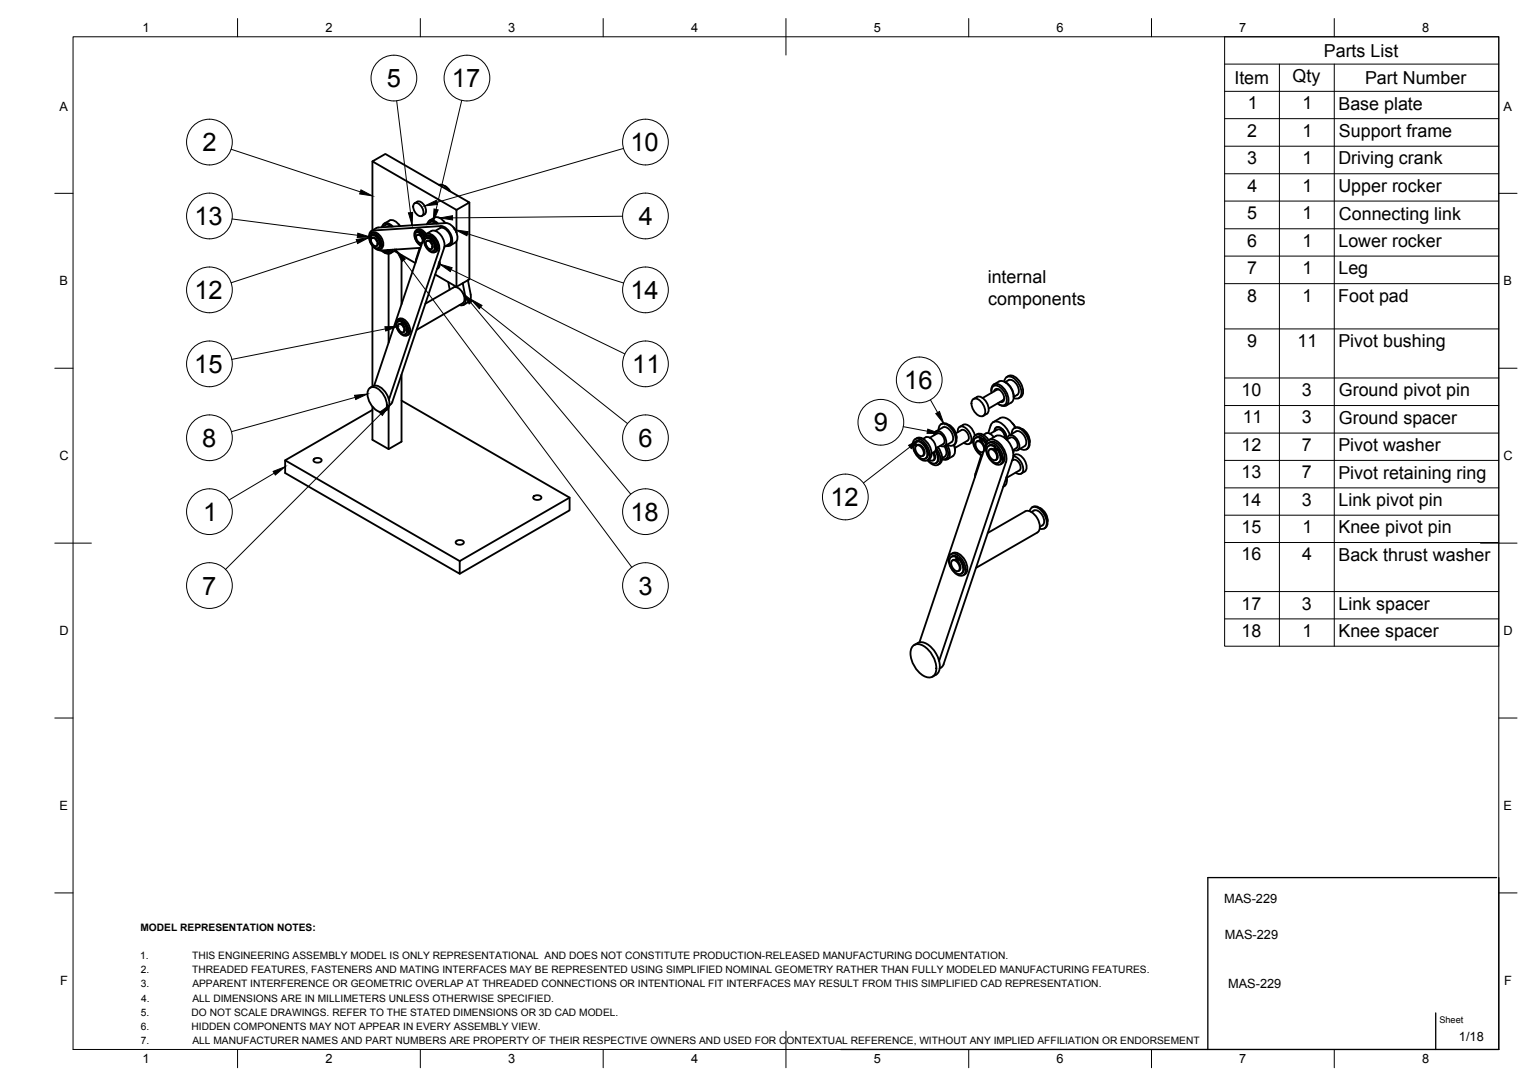
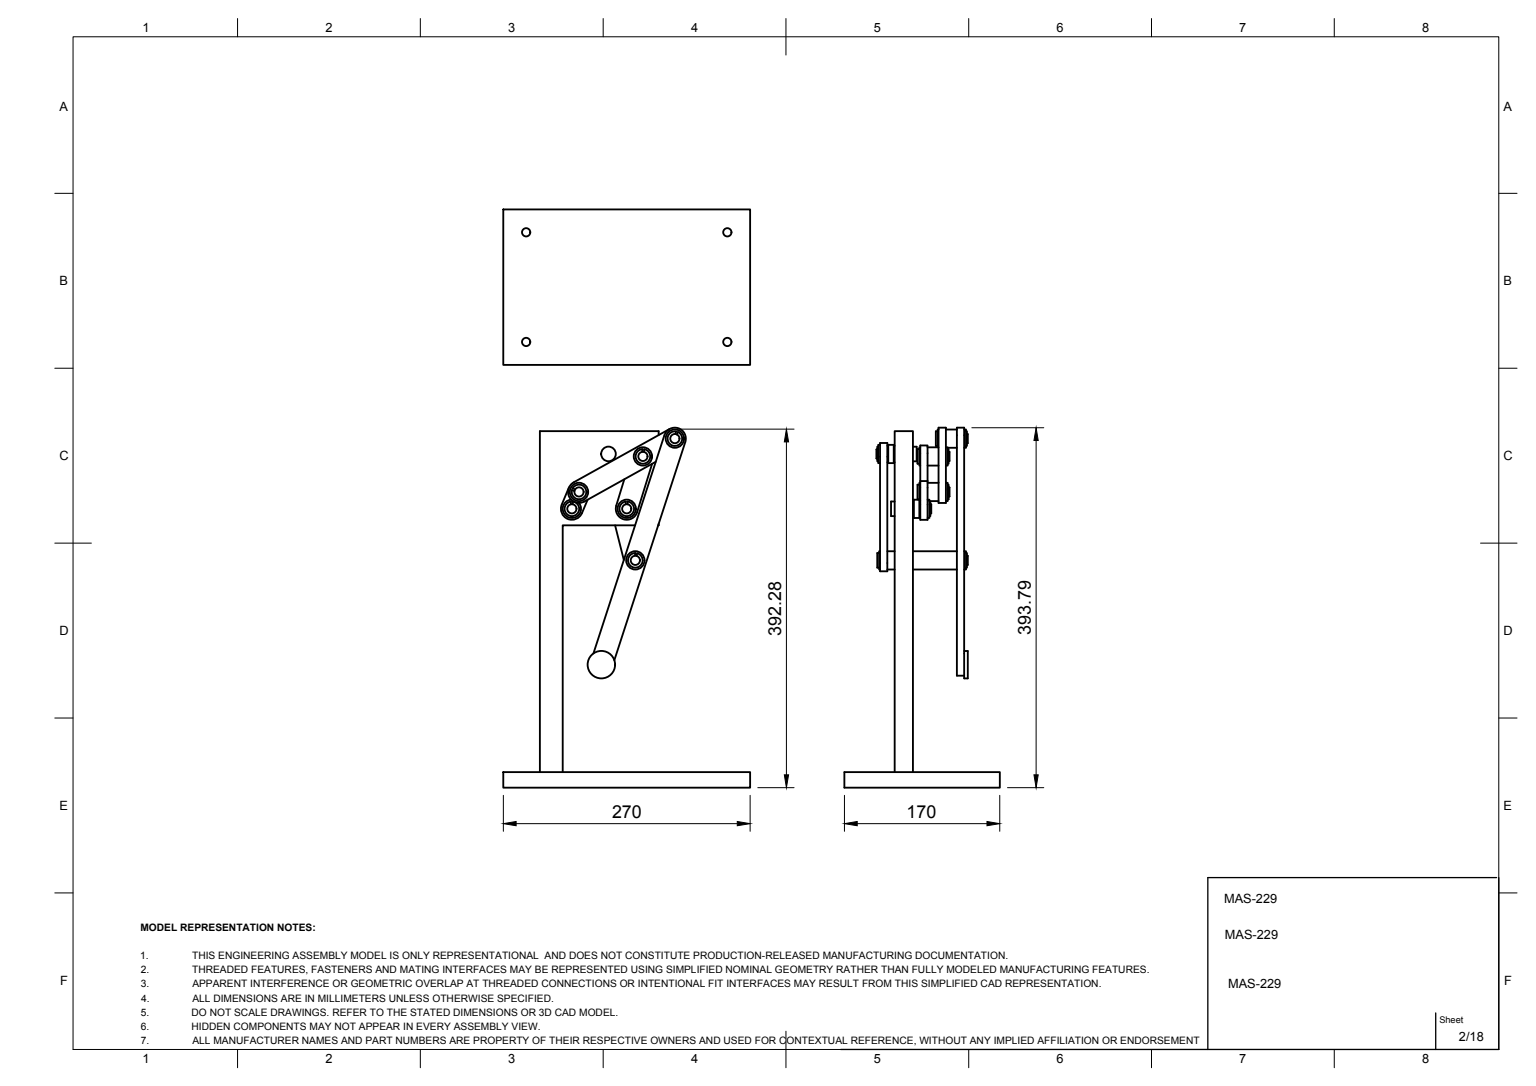
ISO-10303-21;
HEADER;
/* Generated by software containing ST-Developer
 * from STEP Tools, Inc. (www.steptools.com) 
 */

FILE_DESCRIPTION(
/* description */ ('Independently dimensioned six-bar single-leg walking-linkage demonstr
ator. Whole-mm20 crank,60 upper rocker,80/120 ternary coupler,120 lowe
r rocker,140 knee pitch and260 toe reach; ground pivots0/0,60/0,40/60.
 Seven native revolutes close both loops. Four reused native library f
amilies, fully retained shared pins and layered real spacer stacks, bo
nded rubber toe. Benchtop reference mechanism; no complete vehicle, lo
ad, gait stability, adhesive, weld, fit or life rating.'),
/* implementation_level */ '2;1');

FILE_NAME(
/* name */ 'MAS-229.step',
/* time_stamp */ '2026-11-09T20:33:14-08:00',
/* author */ (''),
/* organization */ (''),
/* preprocessor_version */ 'ST-DEVELOPER v20.2',
/* originating_system */ 'Autodesk Translation Framework v15.17.0.0',
/* authorisation */ '');

FILE_SCHEMA (('AUTOMOTIVE_DESIGN { 1 0 10303 214 3 1 1 }'));
ENDSEC;

DATA;
#10=MECHANICAL_DESIGN_GEOMETRIC_PRESENTATION_REPRESENTATION('',(#255,#256,
#257,#258,#259,#260,#261,#262,#263,#264,#265,#266,#267,#268,#269,#270,#271,
#272),#4048);
#11=ITEM_DEFINED_TRANSFORMATION($,$,#2362,#2620);
#12=ITEM_DEFINED_TRANSFORMATION($,$,#2381,#2621);
#13=ITEM_DEFINED_TRANSFORMATION($,$,#2399,#2622);
#14=ITEM_DEFINED_TRANSFORMATION($,$,#2416,#2623);
#15=ITEM_DEFINED_TRANSFORMATION($,$,#2433,#2624);
#16=ITEM_DEFINED_TRANSFORMATION($,$,#2453,#2625);
#17=ITEM_DEFINED_TRANSFORMATION($,$,#2470,#2626);
#18=ITEM_DEFINED_TRANSFORMATION($,$,#2487,#2627);
#19=ITEM_DEFINED_TRANSFORMATION($,$,#2493,#2628);
#20=ITEM_DEFINED_TRANSFORMATION($,$,#2502,#2629);
#21=ITEM_DEFINED_TRANSFORMATION($,$,#2520,#2630);
#22=ITEM_DEFINED_TRANSFORMATION($,$,#2493,#2631);
#23=ITEM_DEFINED_TRANSFORMATION($,$,#2493,#2632);
#24=ITEM_DEFINED_TRANSFORMATION($,$,#2493,#2633);
#25=ITEM_DEFINED_TRANSFORMATION($,$,#2493,#2634);
#26=ITEM_DEFINED_TRANSFORMATION($,$,#2493,#2635);
#27=ITEM_DEFINED_TRANSFORMATION($,$,#2493,#2636);
#28=ITEM_DEFINED_TRANSFORMATION($,$,#2493,#2637);
#29=ITEM_DEFINED_TRANSFORMATION($,$,#2493,#2638);
#30=ITEM_DEFINED_TRANSFORMATION($,$,#2493,#2639);
#31=ITEM_DEFINED_TRANSFORMATION($,$,#2493,#2640);
#32=ITEM_DEFINED_TRANSFORMATION($,$,#2502,#2641);
#33=ITEM_DEFINED_TRANSFORMATION($,$,#2502,#2642);
#34=ITEM_DEFINED_TRANSFORMATION($,$,#2537,#2643);
#35=ITEM_DEFINED_TRANSFORMATION($,$,#2520,#2644);
#36=ITEM_DEFINED_TRANSFORMATION($,$,#2520,#2645);
#37=ITEM_DEFINED_TRANSFORMATION($,$,#2573,#2646);
#38=ITEM_DEFINED_TRANSFORMATION($,$,#2537,#2647);
#39=ITEM_DEFINED_TRANSFORMATION($,$,#2537,#2648);
#40=ITEM_DEFINED_TRANSFORMATION($,$,#2537,#2649);
#41=ITEM_DEFINED_TRANSFORMATION($,$,#2537,#2650);
#42=ITEM_DEFINED_TRANSFORMATION($,$,#2537,#2651);
#43=ITEM_DEFINED_TRANSFORMATION($,$,#2537,#2652);
#44=ITEM_DEFINED_TRANSFORMATION($,$,#2584,#2653);
#45=ITEM_DEFINED_TRANSFORMATION($,$,#2546,#2654);
#46=ITEM_DEFINED_TRANSFORMATION($,$,#2602,#2655);
#47=ITEM_DEFINED_TRANSFORMATION($,$,#2611,#2656);
#48=ITEM_DEFINED_TRANSFORMATION($,$,#2564,#2657);
#49=ITEM_DEFINED_TRANSFORMATION($,$,#2573,#2658);
#50=ITEM_DEFINED_TRANSFORMATION($,$,#2573,#2659);
#51=ITEM_DEFINED_TRANSFORMATION($,$,#2573,#2660);
#52=ITEM_DEFINED_TRANSFORMATION($,$,#2573,#2661);
#53=ITEM_DEFINED_TRANSFORMATION($,$,#2573,#2662);
#54=ITEM_DEFINED_TRANSFORMATION($,$,#2573,#2663);
#55=ITEM_DEFINED_TRANSFORMATION($,$,#2584,#2664);
#56=ITEM_DEFINED_TRANSFORMATION($,$,#2584,#2665);
#57=ITEM_DEFINED_TRANSFORMATION($,$,#2602,#2666);
#58=ITEM_DEFINED_TRANSFORMATION($,$,#2602,#2667);
#59=ITEM_DEFINED_TRANSFORMATION($,$,#2602,#2668);
#60=ITEM_DEFINED_TRANSFORMATION($,$,#2611,#2669);
#61=ITEM_DEFINED_TRANSFORMATION($,$,#2611,#2670);
#62=(
REPRESENTATION_RELATIONSHIP($,$,#4143,#4142)
REPRESENTATION_RELATIONSHIP_WITH_TRANSFORMATION(#11)
SHAPE_REPRESENTATION_RELATIONSHIP()
);
#63=(
REPRESENTATION_RELATIONSHIP($,$,#4144,#4142)
REPRESENTATION_RELATIONSHIP_WITH_TRANSFORMATION(#12)
SHAPE_REPRESENTATION_RELATIONSHIP()
);
#64=(
REPRESENTATION_RELATIONSHIP($,$,#4145,#4142)
REPRESENTATION_RELATIONSHIP_WITH_TRANSFORMATION(#13)
SHAPE_REPRESENTATION_RELATIONSHIP()
);
#65=(
REPRESENTATION_RELATIONSHIP($,$,#4146,#4142)
REPRESENTATION_RELATIONSHIP_WITH_TRANSFORMATION(#14)
SHAPE_REPRESENTATION_RELATIONSHIP()
);
#66=(
REPRESENTATION_RELATIONSHIP($,$,#4147,#4142)
REPRESENTATION_RELATIONSHIP_WITH_TRANSFORMATION(#15)
SHAPE_REPRESENTATION_RELATIONSHIP()
);
#67=(
REPRESENTATION_RELATIONSHIP($,$,#4148,#4142)
REPRESENTATION_RELATIONSHIP_WITH_TRANSFORMATION(#16)
SHAPE_REPRESENTATION_RELATIONSHIP()
);
#68=(
REPRESENTATION_RELATIONSHIP($,$,#4149,#4142)
REPRESENTATION_RELATIONSHIP_WITH_TRANSFORMATION(#17)
SHAPE_REPRESENTATION_RELATIONSHIP()
);
#69=(
REPRESENTATION_RELATIONSHIP($,$,#4150,#4142)
REPRESENTATION_RELATIONSHIP_WITH_TRANSFORMATION(#18)
SHAPE_REPRESENTATION_RELATIONSHIP()
);
#70=(
REPRESENTATION_RELATIONSHIP($,$,#4151,#4142)
REPRESENTATION_RELATIONSHIP_WITH_TRANSFORMATION(#19)
SHAPE_REPRESENTATION_RELATIONSHIP()
);
#71=(
REPRESENTATION_RELATIONSHIP($,$,#4152,#4142)
REPRESENTATION_RELATIONSHIP_WITH_TRANSFORMATION(#20)
SHAPE_REPRESENTATION_RELATIONSHIP()
);
#72=(
REPRESENTATION_RELATIONSHIP($,$,#4153,#4142)
REPRESENTATION_RELATIONSHIP_WITH_TRANSFORMATION(#21)
SHAPE_REPRESENTATION_RELATIONSHIP()
);
#73=(
REPRESENTATION_RELATIONSHIP($,$,#4151,#4142)
REPRESENTATION_RELATIONSHIP_WITH_TRANSFORMATION(#22)
SHAPE_REPRESENTATION_RELATIONSHIP()
);
#74=(
REPRESENTATION_RELATIONSHIP($,$,#4151,#4142)
REPRESENTATION_RELATIONSHIP_WITH_TRANSFORMATION(#23)
SHAPE_REPRESENTATION_RELATIONSHIP()
);
#75=(
REPRESENTATION_RELATIONSHIP($,$,#4151,#4142)
REPRESENTATION_RELATIONSHIP_WITH_TRANSFORMATION(#24)
SHAPE_REPRESENTATION_RELATIONSHIP()
);
#76=(
REPRESENTATION_RELATIONSHIP($,$,#4151,#4142)
REPRESENTATION_RELATIONSHIP_WITH_TRANSFORMATION(#25)
SHAPE_REPRESENTATION_RELATIONSHIP()
);
#77=(
REPRESENTATION_RELATIONSHIP($,$,#4151,#4142)
REPRESENTATION_RELATIONSHIP_WITH_TRANSFORMATION(#26)
SHAPE_REPRESENTATION_RELATIONSHIP()
);
#78=(
REPRESENTATION_RELATIONSHIP($,$,#4151,#4142)
REPRESENTATION_RELATIONSHIP_WITH_TRANSFORMATION(#27)
SHAPE_REPRESENTATION_RELATIONSHIP()
);
#79=(
REPRESENTATION_RELATIONSHIP($,$,#4151,#4142)
REPRESENTATION_RELATIONSHIP_WITH_TRANSFORMATION(#28)
SHAPE_REPRESENTATION_RELATIONSHIP()
);
#80=(
REPRESENTATION_RELATIONSHIP($,$,#4151,#4142)
REPRESENTATION_RELATIONSHIP_WITH_TRANSFORMATION(#29)
SHAPE_REPRESENTATION_RELATIONSHIP()
);
#81=(
REPRESENTATION_RELATIONSHIP($,$,#4151,#4142)
REPRESENTATION_RELATIONSHIP_WITH_TRANSFORMATION(#30)
SHAPE_REPRESENTATION_RELATIONSHIP()
);
#82=(
REPRESENTATION_RELATIONSHIP($,$,#4151,#4142)
REPRESENTATION_RELATIONSHIP_WITH_TRANSFORMATION(#31)
SHAPE_REPRESENTATION_RELATIONSHIP()
);
#83=(
REPRESENTATION_RELATIONSHIP($,$,#4152,#4142)
REPRESENTATION_RELATIONSHIP_WITH_TRANSFORMATION(#32)
SHAPE_REPRESENTATION_RELATIONSHIP()
);
#84=(
REPRESENTATION_RELATIONSHIP($,$,#4152,#4142)
REPRESENTATION_RELATIONSHIP_WITH_TRANSFORMATION(#33)
SHAPE_REPRESENTATION_RELATIONSHIP()
);
#85=(
REPRESENTATION_RELATIONSHIP($,$,#4154,#4142)
REPRESENTATION_RELATIONSHIP_WITH_TRANSFORMATION(#34)
SHAPE_REPRESENTATION_RELATIONSHIP()
);
#86=(
REPRESENTATION_RELATIONSHIP($,$,#4153,#4142)
REPRESENTATION_RELATIONSHIP_WITH_TRANSFORMATION(#35)
SHAPE_REPRESENTATION_RELATIONSHIP()
);
#87=(
REPRESENTATION_RELATIONSHIP($,$,#4153,#4142)
REPRESENTATION_RELATIONSHIP_WITH_TRANSFORMATION(#36)
SHAPE_REPRESENTATION_RELATIONSHIP()
);
#88=(
REPRESENTATION_RELATIONSHIP($,$,#4157,#4142)
REPRESENTATION_RELATIONSHIP_WITH_TRANSFORMATION(#37)
SHAPE_REPRESENTATION_RELATIONSHIP()
);
#89=(
REPRESENTATION_RELATIONSHIP($,$,#4154,#4142)
REPRESENTATION_RELATIONSHIP_WITH_TRANSFORMATION(#38)
SHAPE_REPRESENTATION_RELATIONSHIP()
);
#90=(
REPRESENTATION_RELATIONSHIP($,$,#4154,#4142)
REPRESENTATION_RELATIONSHIP_WITH_TRANSFORMATION(#39)
SHAPE_REPRESENTATION_RELATIONSHIP()
);
#91=(
REPRESENTATION_RELATIONSHIP($,$,#4154,#4142)
REPRESENTATION_RELATIONSHIP_WITH_TRANSFORMATION(#40)
SHAPE_REPRESENTATION_RELATIONSHIP()
);
#92=(
REPRESENTATION_RELATIONSHIP($,$,#4154,#4142)
REPRESENTATION_RELATIONSHIP_WITH_TRANSFORMATION(#41)
SHAPE_REPRESENTATION_RELATIONSHIP()
);
#93=(
REPRESENTATION_RELATIONSHIP($,$,#4154,#4142)
REPRESENTATION_RELATIONSHIP_WITH_TRANSFORMATION(#42)
SHAPE_REPRESENTATION_RELATIONSHIP()
);
#94=(
REPRESENTATION_RELATIONSHIP($,$,#4154,#4142)
REPRESENTATION_RELATIONSHIP_WITH_TRANSFORMATION(#43)
SHAPE_REPRESENTATION_RELATIONSHIP()
);
#95=(
REPRESENTATION_RELATIONSHIP($,$,#4158,#4142)
REPRESENTATION_RELATIONSHIP_WITH_TRANSFORMATION(#44)
SHAPE_REPRESENTATION_RELATIONSHIP()
);
#96=(
REPRESENTATION_RELATIONSHIP($,$,#4155,#4142)
REPRESENTATION_RELATIONSHIP_WITH_TRANSFORMATION(#45)
SHAPE_REPRESENTATION_RELATIONSHIP()
);
#97=(
REPRESENTATION_RELATIONSHIP($,$,#4159,#4142)
REPRESENTATION_RELATIONSHIP_WITH_TRANSFORMATION(#46)
SHAPE_REPRESENTATION_RELATIONSHIP()
);
#98=(
REPRESENTATION_RELATIONSHIP($,$,#4160,#4142)
REPRESENTATION_RELATIONSHIP_WITH_TRANSFORMATION(#47)
SHAPE_REPRESENTATION_RELATIONSHIP()
);
#99=(
REPRESENTATION_RELATIONSHIP($,$,#4156,#4142)
REPRESENTATION_RELATIONSHIP_WITH_TRANSFORMATION(#48)
SHAPE_REPRESENTATION_RELATIONSHIP()
);
#100=(
REPRESENTATION_RELATIONSHIP($,$,#4157,#4142)
REPRESENTATION_RELATIONSHIP_WITH_TRANSFORMATION(#49)
SHAPE_REPRESENTATION_RELATIONSHIP()
);
#101=(
REPRESENTATION_RELATIONSHIP($,$,#4157,#4142)
REPRESENTATION_RELATIONSHIP_WITH_TRANSFORMATION(#50)
SHAPE_REPRESENTATION_RELATIONSHIP()
);
#102=(
REPRESENTATION_RELATIONSHIP($,$,#4157,#4142)
REPRESENTATION_RELATIONSHIP_WITH_TRANSFORMATION(#51)
SHAPE_REPRESENTATION_RELATIONSHIP()
);
#103=(
REPRESENTATION_RELATIONSHIP($,$,#4157,#4142)
REPRESENTATION_RELATIONSHIP_WITH_TRANSFORMATION(#52)
SHAPE_REPRESENTATION_RELATIONSHIP()
);
#104=(
REPRESENTATION_RELATIONSHIP($,$,#4157,#4142)
REPRESENTATION_RELATIONSHIP_WITH_TRANSFORMATION(#53)
SHAPE_REPRESENTATION_RELATIONSHIP()
);
#105=(
REPRESENTATION_RELATIONSHIP($,$,#4157,#4142)
REPRESENTATION_RELATIONSHIP_WITH_TRANSFORMATION(#54)
SHAPE_REPRESENTATION_RELATIONSHIP()
);
#106=(
REPRESENTATION_RELATIONSHIP($,$,#4158,#4142)
REPRESENTATION_RELATIONSHIP_WITH_TRANSFORMATION(#55)
SHAPE_REPRESENTATION_RELATIONSHIP()
);
#107=(
REPRESENTATION_RELATIONSHIP($,$,#4158,#4142)
REPRESENTATION_RELATIONSHIP_WITH_TRANSFORMATION(#56)
SHAPE_REPRESENTATION_RELATIONSHIP()
);
#108=(
REPRESENTATION_RELATIONSHIP($,$,#4159,#4142)
REPRESENTATION_RELATIONSHIP_WITH_TRANSFORMATION(#57)
SHAPE_REPRESENTATION_RELATIONSHIP()
);
#109=(
REPRESENTATION_RELATIONSHIP($,$,#4159,#4142)
REPRESENTATION_RELATIONSHIP_WITH_TRANSFORMATION(#58)
SHAPE_REPRESENTATION_RELATIONSHIP()
);
#110=(
REPRESENTATION_RELATIONSHIP($,$,#4159,#4142)
REPRESENTATION_RELATIONSHIP_WITH_TRANSFORMATION(#59)
SHAPE_REPRESENTATION_RELATIONSHIP()
);
#111=(
REPRESENTATION_RELATIONSHIP($,$,#4160,#4142)
REPRESENTATION_RELATIONSHIP_WITH_TRANSFORMATION(#60)
SHAPE_REPRESENTATION_RELATIONSHIP()
);
#112=(
REPRESENTATION_RELATIONSHIP($,$,#4160,#4142)
REPRESENTATION_RELATIONSHIP_WITH_TRANSFORMATION(#61)
SHAPE_REPRESENTATION_RELATIONSHIP()
);
#113=CONTEXT_DEPENDENT_SHAPE_REPRESENTATION(#62,#4091);
#114=CONTEXT_DEPENDENT_SHAPE_REPRESENTATION(#63,#4092);
#115=CONTEXT_DEPENDENT_SHAPE_REPRESENTATION(#64,#4093);
#116=CONTEXT_DEPENDENT_SHAPE_REPRESENTATION(#65,#4094);
#117=CONTEXT_DEPENDENT_SHAPE_REPRESENTATION(#66,#4095);
#118=CONTEXT_DEPENDENT_SHAPE_REPRESENTATION(#67,#4096);
#119=CONTEXT_DEPENDENT_SHAPE_REPRESENTATION(#68,#4097);
#120=CONTEXT_DEPENDENT_SHAPE_REPRESENTATION(#69,#4098);
#121=CONTEXT_DEPENDENT_SHAPE_REPRESENTATION(#70,#4099);
#122=CONTEXT_DEPENDENT_SHAPE_REPRESENTATION(#71,#4100);
#123=CONTEXT_DEPENDENT_SHAPE_REPRESENTATION(#72,#4101);
#124=CONTEXT_DEPENDENT_SHAPE_REPRESENTATION(#73,#4102);
#125=CONTEXT_DEPENDENT_SHAPE_REPRESENTATION(#74,#4103);
#126=CONTEXT_DEPENDENT_SHAPE_REPRESENTATION(#75,#4104);
#127=CONTEXT_DEPENDENT_SHAPE_REPRESENTATION(#76,#4105);
#128=CONTEXT_DEPENDENT_SHAPE_REPRESENTATION(#77,#4106);
#129=CONTEXT_DEPENDENT_SHAPE_REPRESENTATION(#78,#4107);
#130=CONTEXT_DEPENDENT_SHAPE_REPRESENTATION(#79,#4108);
#131=CONTEXT_DEPENDENT_SHAPE_REPRESENTATION(#80,#4109);
#132=CONTEXT_DEPENDENT_SHAPE_REPRESENTATION(#81,#4110);
#133=CONTEXT_DEPENDENT_SHAPE_REPRESENTATION(#82,#4111);
#134=CONTEXT_DEPENDENT_SHAPE_REPRESENTATION(#83,#4112);
#135=CONTEXT_DEPENDENT_SHAPE_REPRESENTATION(#84,#4113);
#136=CONTEXT_DEPENDENT_SHAPE_REPRESENTATION(#85,#4114);
#137=CONTEXT_DEPENDENT_SHAPE_REPRESENTATION(#86,#4115);
#138=CONTEXT_DEPENDENT_SHAPE_REPRESENTATION(#87,#4116);
#139=CONTEXT_DEPENDENT_SHAPE_REPRESENTATION(#88,#4117);
#140=CONTEXT_DEPENDENT_SHAPE_REPRESENTATION(#89,#4118);
#141=CONTEXT_DEPENDENT_SHAPE_REPRESENTATION(#90,#4119);
#142=CONTEXT_DEPENDENT_SHAPE_REPRESENTATION(#91,#4120);
#143=CONTEXT_DEPENDENT_SHAPE_REPRESENTATION(#92,#4121);
#144=CONTEXT_DEPENDENT_SHAPE_REPRESENTATION(#93,#4122);
#145=CONTEXT_DEPENDENT_SHAPE_REPRESENTATION(#94,#4123);
#146=CONTEXT_DEPENDENT_SHAPE_REPRESENTATION(#95,#4124);
#147=CONTEXT_DEPENDENT_SHAPE_REPRESENTATION(#96,#4125);
#148=CONTEXT_DEPENDENT_SHAPE_REPRESENTATION(#97,#4126);
#149=CONTEXT_DEPENDENT_SHAPE_REPRESENTATION(#98,#4127);
#150=CONTEXT_DEPENDENT_SHAPE_REPRESENTATION(#99,#4128);
#151=CONTEXT_DEPENDENT_SHAPE_REPRESENTATION(#100,#4129);
#152=CONTEXT_DEPENDENT_SHAPE_REPRESENTATION(#101,#4130);
#153=CONTEXT_DEPENDENT_SHAPE_REPRESENTATION(#102,#4131);
#154=CONTEXT_DEPENDENT_SHAPE_REPRESENTATION(#103,#4132);
#155=CONTEXT_DEPENDENT_SHAPE_REPRESENTATION(#104,#4133);
#156=CONTEXT_DEPENDENT_SHAPE_REPRESENTATION(#105,#4134);
#157=CONTEXT_DEPENDENT_SHAPE_REPRESENTATION(#106,#4135);
#158=CONTEXT_DEPENDENT_SHAPE_REPRESENTATION(#107,#4136);
#159=CONTEXT_DEPENDENT_SHAPE_REPRESENTATION(#108,#4137);
#160=CONTEXT_DEPENDENT_SHAPE_REPRESENTATION(#109,#4138);
#161=CONTEXT_DEPENDENT_SHAPE_REPRESENTATION(#110,#4139);
#162=CONTEXT_DEPENDENT_SHAPE_REPRESENTATION(#111,#4140);
#163=CONTEXT_DEPENDENT_SHAPE_REPRESENTATION(#112,#4141);
#164=NEXT_ASSEMBLY_USAGE_OCCURRENCE('Base plate:1','Base plate:1',
'Base plate:1',#4162,#4163,'Base plate:1');
#165=NEXT_ASSEMBLY_USAGE_OCCURRENCE('Support frame:1','Support frame:1',
'Support frame:1',#4162,#4164,'Support frame:1');
#166=NEXT_ASSEMBLY_USAGE_OCCURRENCE('Driving crank:1','Driving crank:1',
'Driving crank:1',#4162,#4165,'Driving crank:1');
#167=NEXT_ASSEMBLY_USAGE_OCCURRENCE('Upper rocker:1','Upper rocker:1',
'Upper rocker:1',#4162,#4166,'Upper rocker:1');
#168=NEXT_ASSEMBLY_USAGE_OCCURRENCE('Connecting link:1',
'Connecting link:1','Connecting link:1',#4162,#4167,'Connecting link:1');
#169=NEXT_ASSEMBLY_USAGE_OCCURRENCE('Lower rocker:1','Lower rocker:1',
'Lower rocker:1',#4162,#4168,'Lower rocker:1');
#170=NEXT_ASSEMBLY_USAGE_OCCURRENCE('Leg:1','Leg:1','Leg:1',#4162,#4169,
'Leg:1');
#171=NEXT_ASSEMBLY_USAGE_OCCURRENCE('Foot pad:1','Foot pad:1',
'Foot pad:1',#4162,#4170,'Foot pad:1');
#172=NEXT_ASSEMBLY_USAGE_OCCURRENCE('Pivot bushing:1','Pivot bushing:1',
'Pivot bushing:1',#4162,#4171,'Pivot bushing:1');
#173=NEXT_ASSEMBLY_USAGE_OCCURRENCE('Ground pivot pin:1',
'Ground pivot pin:1','Ground pivot pin:1',#4162,#4172,
'Ground pivot pin:1');
#174=NEXT_ASSEMBLY_USAGE_OCCURRENCE('Ground spacer:1','Ground spacer:1',
'Ground spacer:1',#4162,#4173,'Ground spacer:1');
#175=NEXT_ASSEMBLY_USAGE_OCCURRENCE('Pivot bushing:2','Pivot bushing:2',
'Pivot bushing:2',#4162,#4171,'Pivot bushing:2');
#176=NEXT_ASSEMBLY_USAGE_OCCURRENCE('Pivot bushing:3','Pivot bushing:3',
'Pivot bushing:3',#4162,#4171,'Pivot bushing:3');
#177=NEXT_ASSEMBLY_USAGE_OCCURRENCE('Pivot bushing:4','Pivot bushing:4',
'Pivot bushing:4',#4162,#4171,'Pivot bushing:4');
#178=NEXT_ASSEMBLY_USAGE_OCCURRENCE('Pivot bushing:5','Pivot bushing:5',
'Pivot bushing:5',#4162,#4171,'Pivot bushing:5');
#179=NEXT_ASSEMBLY_USAGE_OCCURRENCE('Pivot bushing:6','Pivot bushing:6',
'Pivot bushing:6',#4162,#4171,'Pivot bushing:6');
#180=NEXT_ASSEMBLY_USAGE_OCCURRENCE('Pivot bushing:7','Pivot bushing:7',
'Pivot bushing:7',#4162,#4171,'Pivot bushing:7');
#181=NEXT_ASSEMBLY_USAGE_OCCURRENCE('Pivot bushing:8','Pivot bushing:8',
'Pivot bushing:8',#4162,#4171,'Pivot bushing:8');
#182=NEXT_ASSEMBLY_USAGE_OCCURRENCE('Pivot bushing:9','Pivot bushing:9',
'Pivot bushing:9',#4162,#4171,'Pivot bushing:9');
#183=NEXT_ASSEMBLY_USAGE_OCCURRENCE('Pivot bushing:10',
'Pivot bushing:10','Pivot bushing:10',#4162,#4171,'Pivot bushing:10');
#184=NEXT_ASSEMBLY_USAGE_OCCURRENCE('Pivot bushing:11',
'Pivot bushing:11','Pivot bushing:11',#4162,#4171,'Pivot bushing:11');
#185=NEXT_ASSEMBLY_USAGE_OCCURRENCE('Ground pivot pin:2',
'Ground pivot pin:2','Ground pivot pin:2',#4162,#4172,
'Ground pivot pin:2');
#186=NEXT_ASSEMBLY_USAGE_OCCURRENCE('Ground pivot pin:3',
'Ground pivot pin:3','Ground pivot pin:3',#4162,#4172,
'Ground pivot pin:3');
#187=NEXT_ASSEMBLY_USAGE_OCCURRENCE('Pivot washer:1','Pivot washer:1',
'Pivot washer:1',#4162,#4174,'Pivot washer:1');
#188=NEXT_ASSEMBLY_USAGE_OCCURRENCE('Ground spacer:2','Ground spacer:2',
'Ground spacer:2',#4162,#4173,'Ground spacer:2');
#189=NEXT_ASSEMBLY_USAGE_OCCURRENCE('Ground spacer:3','Ground spacer:3',
'Ground spacer:3',#4162,#4173,'Ground spacer:3');
#190=NEXT_ASSEMBLY_USAGE_OCCURRENCE('Pivot retaining ring:1',
'Pivot retaining ring:1','Pivot retaining ring:1',#4162,#4177,
'Pivot retaining ring:1');
#191=NEXT_ASSEMBLY_USAGE_OCCURRENCE('Pivot washer:2','Pivot washer:2',
'Pivot washer:2',#4162,#4174,'Pivot washer:2');
#192=NEXT_ASSEMBLY_USAGE_OCCURRENCE('Pivot washer:3','Pivot washer:3',
'Pivot washer:3',#4162,#4174,'Pivot washer:3');
#193=NEXT_ASSEMBLY_USAGE_OCCURRENCE('Pivot washer:4','Pivot washer:4',
'Pivot washer:4',#4162,#4174,'Pivot washer:4');
#194=NEXT_ASSEMBLY_USAGE_OCCURRENCE('Pivot washer:5','Pivot washer:5',
'Pivot washer:5',#4162,#4174,'Pivot washer:5');
#195=NEXT_ASSEMBLY_USAGE_OCCURRENCE('Pivot washer:6','Pivot washer:6',
'Pivot washer:6',#4162,#4174,'Pivot washer:6');
#196=NEXT_ASSEMBLY_USAGE_OCCURRENCE('Pivot washer:7','Pivot washer:7',
'Pivot washer:7',#4162,#4174,'Pivot washer:7');
#197=NEXT_ASSEMBLY_USAGE_OCCURRENCE('Link pivot pin:1',
'Link pivot pin:1','Link pivot pin:1',#4162,#4178,'Link pivot pin:1');
#198=NEXT_ASSEMBLY_USAGE_OCCURRENCE('Knee pivot pin:1',
'Knee pivot pin:1','Knee pivot pin:1',#4162,#4175,'Knee pivot pin:1');
#199=NEXT_ASSEMBLY_USAGE_OCCURRENCE('Back thrust washer:1',
'Back thrust washer:1','Back thrust washer:1',#4162,#4179,
'Back thrust washer:1');
#200=NEXT_ASSEMBLY_USAGE_OCCURRENCE('Link spacer:1','Link spacer:1',
'Link spacer:1',#4162,#4180,'Link spacer:1');
#201=NEXT_ASSEMBLY_USAGE_OCCURRENCE('Knee spacer:1','Knee spacer:1',
'Knee spacer:1',#4162,#4176,'Knee spacer:1');
#202=NEXT_ASSEMBLY_USAGE_OCCURRENCE('Pivot retaining ring:2',
'Pivot retaining ring:2','Pivot retaining ring:2',#4162,#4177,
'Pivot retaining ring:2');
#203=NEXT_ASSEMBLY_USAGE_OCCURRENCE('Pivot retaining ring:3',
'Pivot retaining ring:3','Pivot retaining ring:3',#4162,#4177,
'Pivot retaining ring:3');
#204=NEXT_ASSEMBLY_USAGE_OCCURRENCE('Pivot retaining ring:4',
'Pivot retaining ring:4','Pivot retaining ring:4',#4162,#4177,
'Pivot retaining ring:4');
#205=NEXT_ASSEMBLY_USAGE_OCCURRENCE('Pivot retaining ring:5',
'Pivot retaining ring:5','Pivot retaining ring:5',#4162,#4177,
'Pivot retaining ring:5');
#206=NEXT_ASSEMBLY_USAGE_OCCURRENCE('Pivot retaining ring:6',
'Pivot retaining ring:6','Pivot retaining ring:6',#4162,#4177,
'Pivot retaining ring:6');
#207=NEXT_ASSEMBLY_USAGE_OCCURRENCE('Pivot retaining ring:7',
'Pivot retaining ring:7','Pivot retaining ring:7',#4162,#4177,
'Pivot retaining ring:7');
#208=NEXT_ASSEMBLY_USAGE_OCCURRENCE('Link pivot pin:2',
'Link pivot pin:2','Link pivot pin:2',#4162,#4178,'Link pivot pin:2');
#209=NEXT_ASSEMBLY_USAGE_OCCURRENCE('Link pivot pin:3',
'Link pivot pin:3','Link pivot pin:3',#4162,#4178,'Link pivot pin:3');
#210=NEXT_ASSEMBLY_USAGE_OCCURRENCE('Back thrust washer:2',
'Back thrust washer:2','Back thrust washer:2',#4162,#4179,
'Back thrust washer:2');
#211=NEXT_ASSEMBLY_USAGE_OCCURRENCE('Back thrust washer:3',
'Back thrust washer:3','Back thrust washer:3',#4162,#4179,
'Back thrust washer:3');
#212=NEXT_ASSEMBLY_USAGE_OCCURRENCE('Back thrust washer:4',
'Back thrust washer:4','Back thrust washer:4',#4162,#4179,
'Back thrust washer:4');
#213=NEXT_ASSEMBLY_USAGE_OCCURRENCE('Link spacer:2','Link spacer:2',
'Link spacer:2',#4162,#4180,'Link spacer:2');
#214=NEXT_ASSEMBLY_USAGE_OCCURRENCE('Link spacer:3','Link spacer:3',
'Link spacer:3',#4162,#4180,'Link spacer:3');
#215=CONICAL_SURFACE('',#2521,9.5,0.785398163397448);
#216=CONICAL_SURFACE('',#2528,9.5,0.785398163397448);
#217=CONICAL_SURFACE('',#2532,5.5,0.785398163397448);
#218=CONICAL_SURFACE('',#2536,5.5,0.785398163397448);
#219=SHAPE_REPRESENTATION_RELATIONSHIP('SRR','None',#4143,#237);
#220=SHAPE_REPRESENTATION_RELATIONSHIP('SRR','None',#4144,#238);
#221=SHAPE_REPRESENTATION_RELATIONSHIP('SRR','None',#4145,#239);
#222=SHAPE_REPRESENTATION_RELATIONSHIP('SRR','None',#4146,#240);
#223=SHAPE_REPRESENTATION_RELATIONSHIP('SRR','None',#4147,#241);
#224=SHAPE_REPRESENTATION_RELATIONSHIP('SRR','None',#4148,#242);
#225=SHAPE_REPRESENTATION_RELATIONSHIP('SRR','None',#4149,#243);
#226=SHAPE_REPRESENTATION_RELATIONSHIP('SRR','None',#4150,#244);
#227=SHAPE_REPRESENTATION_RELATIONSHIP('SRR','None',#4151,#245);
#228=SHAPE_REPRESENTATION_RELATIONSHIP('SRR','None',#4152,#246);
#229=SHAPE_REPRESENTATION_RELATIONSHIP('SRR','None',#4153,#247);
#230=SHAPE_REPRESENTATION_RELATIONSHIP('SRR','None',#4154,#248);
#231=SHAPE_REPRESENTATION_RELATIONSHIP('SRR','None',#4155,#249);
#232=SHAPE_REPRESENTATION_RELATIONSHIP('SRR','None',#4156,#250);
#233=SHAPE_REPRESENTATION_RELATIONSHIP('SRR','None',#4157,#251);
#234=SHAPE_REPRESENTATION_RELATIONSHIP('SRR','None',#4158,#252);
#235=SHAPE_REPRESENTATION_RELATIONSHIP('SRR','None',#4159,#253);
#236=SHAPE_REPRESENTATION_RELATIONSHIP('SRR','None',#4160,#254);
#237=ADVANCED_BREP_SHAPE_REPRESENTATION('',(#273),#4030);
#238=ADVANCED_BREP_SHAPE_REPRESENTATION('',(#274),#4031);
#239=ADVANCED_BREP_SHAPE_REPRESENTATION('',(#275),#4032);
#240=ADVANCED_BREP_SHAPE_REPRESENTATION('',(#276),#4033);
#241=ADVANCED_BREP_SHAPE_REPRESENTATION('',(#277),#4034);
#242=ADVANCED_BREP_SHAPE_REPRESENTATION('',(#278),#4035);
#243=ADVANCED_BREP_SHAPE_REPRESENTATION('',(#279),#4036);
#244=ADVANCED_BREP_SHAPE_REPRESENTATION('',(#280),#4037);
#245=ADVANCED_BREP_SHAPE_REPRESENTATION('',(#281),#4038);
#246=ADVANCED_BREP_SHAPE_REPRESENTATION('',(#282),#4039);
#247=ADVANCED_BREP_SHAPE_REPRESENTATION('',(#283),#4040);
#248=ADVANCED_BREP_SHAPE_REPRESENTATION('',(#284),#4041);
#249=ADVANCED_BREP_SHAPE_REPRESENTATION('',(#285),#4042);
#250=ADVANCED_BREP_SHAPE_REPRESENTATION('',(#286),#4043);
#251=ADVANCED_BREP_SHAPE_REPRESENTATION('',(#287),#4044);
#252=ADVANCED_BREP_SHAPE_REPRESENTATION('',(#288),#4045);
#253=ADVANCED_BREP_SHAPE_REPRESENTATION('',(#289),#4046);
#254=ADVANCED_BREP_SHAPE_REPRESENTATION('',(#290),#4047);
#255=STYLED_ITEM('',(#4242),#273);
#256=STYLED_ITEM('',(#4243),#274);
#257=STYLED_ITEM('',(#4244),#275);
#258=STYLED_ITEM('',(#4245),#276);
#259=STYLED_ITEM('',(#4246),#277);
#260=STYLED_ITEM('',(#4247),#278);
#261=STYLED_ITEM('',(#4248),#279);
#262=STYLED_ITEM('',(#4249),#280);
#263=STYLED_ITEM('',(#4250),#281);
#264=STYLED_ITEM('',(#4251),#282);
#265=STYLED_ITEM('',(#4241),#283);
#266=STYLED_ITEM('',(#4252),#284);
#267=STYLED_ITEM('',(#4251),#285);
#268=STYLED_ITEM('',(#4253),#286);
#269=STYLED_ITEM('',(#4254),#287);
#270=STYLED_ITEM('',(#4251),#288);
#271=STYLED_ITEM('',(#4250),#289);
#272=STYLED_ITEM('',(#4253),#290);
#273=MANIFOLD_SOLID_BREP('Body1',#2144);
#274=MANIFOLD_SOLID_BREP('Body1',#2145);
#275=MANIFOLD_SOLID_BREP('Body1',#2146);
#276=MANIFOLD_SOLID_BREP('Body1',#2147);
#277=MANIFOLD_SOLID_BREP('Body1',#2148);
#278=MANIFOLD_SOLID_BREP('Body1',#2149);
#279=MANIFOLD_SOLID_BREP('Body1',#2150);
#280=MANIFOLD_SOLID_BREP('Body1',#2151);
#281=MANIFOLD_SOLID_BREP('Body1',#2152);
#282=MANIFOLD_SOLID_BREP('Body1',#2153);
#283=MANIFOLD_SOLID_BREP('Spacer',#2154);
#284=MANIFOLD_SOLID_BREP('Body1',#2155);
#285=MANIFOLD_SOLID_BREP('Body1',#2156);
#286=MANIFOLD_SOLID_BREP('Body1',#2157);
#287=MANIFOLD_SOLID_BREP('Body1',#2158);
#288=MANIFOLD_SOLID_BREP('Body1',#2159);
#289=MANIFOLD_SOLID_BREP('Body1',#2160);
#290=MANIFOLD_SOLID_BREP('Body1',#2161);
#291=FACE_BOUND('',#550,.T.);
#292=FACE_BOUND('',#551,.T.);
#293=FACE_BOUND('',#552,.T.);
#294=FACE_BOUND('',#553,.T.);
#295=FACE_BOUND('',#555,.T.);
#296=FACE_BOUND('',#556,.T.);
#297=FACE_BOUND('',#557,.T.);
#298=FACE_BOUND('',#558,.T.);
#299=FACE_BOUND('',#569,.T.);
#300=FACE_BOUND('',#570,.T.);
#301=FACE_BOUND('',#571,.T.);
#302=FACE_BOUND('',#573,.T.);
#303=FACE_BOUND('',#574,.T.);
#304=FACE_BOUND('',#575,.T.);
#305=FACE_BOUND('',#583,.T.);
#306=FACE_BOUND('',#584,.T.);
#307=FACE_BOUND('',#586,.T.);
#308=FACE_BOUND('',#587,.T.);
#309=FACE_BOUND('',#595,.T.);
#310=FACE_BOUND('',#596,.T.);
#311=FACE_BOUND('',#598,.T.);
#312=FACE_BOUND('',#599,.T.);
#313=FACE_BOUND('',#608,.T.);
#314=FACE_BOUND('',#609,.T.);
#315=FACE_BOUND('',#610,.T.);
#316=FACE_BOUND('',#612,.T.);
#317=FACE_BOUND('',#613,.T.);
#318=FACE_BOUND('',#614,.T.);
#319=FACE_BOUND('',#622,.T.);
#320=FACE_BOUND('',#623,.T.);
#321=FACE_BOUND('',#625,.T.);
#322=FACE_BOUND('',#626,.T.);
#323=FACE_BOUND('',#634,.T.);
#324=FACE_BOUND('',#635,.T.);
#325=FACE_BOUND('',#637,.T.);
#326=FACE_BOUND('',#638,.T.);
#327=FACE_BOUND('',#645,.T.);
#328=FACE_BOUND('',#647,.T.);
#329=FACE_BOUND('',#650,.T.);
#330=FACE_BOUND('',#652,.T.);
#331=FACE_BOUND('',#655,.T.);
#332=FACE_BOUND('',#663,.T.);
#333=FACE_BOUND('',#666,.T.);
#334=FACE_BOUND('',#673,.T.);
#335=FACE_BOUND('',#675,.T.);
#336=FACE_BOUND('',#678,.T.);
#337=FACE_BOUND('',#680,.T.);
#338=FACE_BOUND('',#683,.T.);
#339=FACE_BOUND('',#691,.T.);
#340=FACE_BOUND('',#693,.T.);
#341=FACE_BOUND('',#702,.T.);
#342=FACE_BOUND('',#704,.T.);
#343=FACE_BOUND('',#707,.T.);
#344=FACE_BOUND('',#715,.T.);
#345=FACE_BOUND('',#717,.T.);
#346=FACE_BOUND('',#721,.T.);
#347=FACE_BOUND('',#723,.T.);
#348=PLANE('',#2375);
#349=PLANE('',#2376);
#350=PLANE('',#2377);
#351=PLANE('',#2378);
#352=PLANE('',#2379);
#353=PLANE('',#2380);
#354=PLANE('',#2391);
#355=PLANE('',#2392);
#356=PLANE('',#2393);
#357=PLANE('',#2394);
#358=PLANE('',#2395);
#359=PLANE('',#2396);
#360=PLANE('',#2397);
#361=PLANE('',#2398);
#362=PLANE('',#2406);
#363=PLANE('',#2410);
#364=PLANE('',#2414);
#365=PLANE('',#2415);
#366=PLANE('',#2423);
#367=PLANE('',#2427);
#368=PLANE('',#2431);
#369=PLANE('',#2432);
#370=PLANE('',#2443);
#371=PLANE('',#2447);
#372=PLANE('',#2451);
#373=PLANE('',#2452);
#374=PLANE('',#2460);
#375=PLANE('',#2464);
#376=PLANE('',#2468);
#377=PLANE('',#2469);
#378=PLANE('',#2477);
#379=PLANE('',#2481);
#380=PLANE('',#2485);
#381=PLANE('',#2486);
#382=PLANE('',#2491);
#383=PLANE('',#2492);
#384=PLANE('',#2500);
#385=PLANE('',#2501);
#386=PLANE('',#2506);
#387=PLANE('',#2508);
#388=PLANE('',#2512);
#389=PLANE('',#2517);
#390=PLANE('',#2519);
#391=PLANE('',#2526);
#392=PLANE('',#2530);
#393=PLANE('',#2544);
#394=PLANE('',#2545);
#395=PLANE('',#2550);
#396=PLANE('',#2552);
#397=PLANE('',#2556);
#398=PLANE('',#2561);
#399=PLANE('',#2563);
#400=PLANE('',#2571);
#401=PLANE('',#2572);
#402=PLANE('',#2574);
#403=PLANE('',#2575);
#404=PLANE('',#2576);
#405=PLANE('',#2583);
#406=PLANE('',#2588);
#407=PLANE('',#2590);
#408=PLANE('',#2594);
#409=PLANE('',#2599);
#410=PLANE('',#2601);
#411=PLANE('',#2609);
#412=PLANE('',#2610);
#413=PLANE('',#2618);
#414=PLANE('',#2619);
#415=FACE_OUTER_BOUND('',#541,.T.);
#416=FACE_OUTER_BOUND('',#542,.T.);
#417=FACE_OUTER_BOUND('',#543,.T.);
#418=FACE_OUTER_BOUND('',#544,.T.);
#419=FACE_OUTER_BOUND('',#545,.T.);
#420=FACE_OUTER_BOUND('',#546,.T.);
#421=FACE_OUTER_BOUND('',#547,.T.);
#422=FACE_OUTER_BOUND('',#548,.T.);
#423=FACE_OUTER_BOUND('',#549,.T.);
#424=FACE_OUTER_BOUND('',#554,.T.);
#425=FACE_OUTER_BOUND('',#559,.T.);
#426=FACE_OUTER_BOUND('',#560,.T.);
#427=FACE_OUTER_BOUND('',#561,.T.);
#428=FACE_OUTER_BOUND('',#562,.T.);
#429=FACE_OUTER_BOUND('',#563,.T.);
#430=FACE_OUTER_BOUND('',#564,.T.);
#431=FACE_OUTER_BOUND('',#565,.T.);
#432=FACE_OUTER_BOUND('',#566,.T.);
#433=FACE_OUTER_BOUND('',#567,.T.);
#434=FACE_OUTER_BOUND('',#568,.T.);
#435=FACE_OUTER_BOUND('',#572,.T.);
#436=FACE_OUTER_BOUND('',#576,.T.);
#437=FACE_OUTER_BOUND('',#577,.T.);
#438=FACE_OUTER_BOUND('',#578,.T.);
#439=FACE_OUTER_BOUND('',#579,.T.);
#440=FACE_OUTER_BOUND('',#580,.T.);
#441=FACE_OUTER_BOUND('',#581,.T.);
#442=FACE_OUTER_BOUND('',#582,.T.);
#443=FACE_OUTER_BOUND('',#585,.T.);
#444=FACE_OUTER_BOUND('',#588,.T.);
#445=FACE_OUTER_BOUND('',#589,.T.);
#446=FACE_OUTER_BOUND('',#590,.T.);
#447=FACE_OUTER_BOUND('',#591,.T.);
#448=FACE_OUTER_BOUND('',#592,.T.);
#449=FACE_OUTER_BOUND('',#593,.T.);
#450=FACE_OUTER_BOUND('',#594,.T.);
#451=FACE_OUTER_BOUND('',#597,.T.);
#452=FACE_OUTER_BOUND('',#600,.T.);
#453=FACE_OUTER_BOUND('',#601,.T.);
#454=FACE_OUTER_BOUND('',#602,.T.);
#455=FACE_OUTER_BOUND('',#603,.T.);
#456=FACE_OUTER_BOUND('',#604,.T.);
#457=FACE_OUTER_BOUND('',#605,.T.);
#458=FACE_OUTER_BOUND('',#606,.T.);
#459=FACE_OUTER_BOUND('',#607,.T.);
#460=FACE_OUTER_BOUND('',#611,.T.);
#461=FACE_OUTER_BOUND('',#615,.T.);
#462=FACE_OUTER_BOUND('',#616,.T.);
#463=FACE_OUTER_BOUND('',#617,.T.);
#464=FACE_OUTER_BOUND('',#618,.T.);
#465=FACE_OUTER_BOUND('',#619,.T.);
#466=FACE_OUTER_BOUND('',#620,.T.);
#467=FACE_OUTER_BOUND('',#621,.T.);
#468=FACE_OUTER_BOUND('',#624,.T.);
#469=FACE_OUTER_BOUND('',#627,.T.);
#470=FACE_OUTER_BOUND('',#628,.T.);
#471=FACE_OUTER_BOUND('',#629,.T.);
#472=FACE_OUTER_BOUND('',#630,.T.);
#473=FACE_OUTER_BOUND('',#631,.T.);
#474=FACE_OUTER_BOUND('',#632,.T.);
#475=FACE_OUTER_BOUND('',#633,.T.);
#476=FACE_OUTER_BOUND('',#636,.T.);
#477=FACE_OUTER_BOUND('',#639,.T.);
#478=FACE_OUTER_BOUND('',#640,.T.);
#479=FACE_OUTER_BOUND('',#641,.T.);
#480=FACE_OUTER_BOUND('',#642,.T.);
#481=FACE_OUTER_BOUND('',#643,.T.);
#482=FACE_OUTER_BOUND('',#644,.T.);
#483=FACE_OUTER_BOUND('',#646,.T.);
#484=FACE_OUTER_BOUND('',#648,.T.);
#485=FACE_OUTER_BOUND('',#649,.T.);
#486=FACE_OUTER_BOUND('',#651,.T.);
#487=FACE_OUTER_BOUND('',#653,.T.);
#488=FACE_OUTER_BOUND('',#654,.T.);
#489=FACE_OUTER_BOUND('',#656,.T.);
#490=FACE_OUTER_BOUND('',#657,.T.);
#491=FACE_OUTER_BOUND('',#658,.T.);
#492=FACE_OUTER_BOUND('',#659,.T.);
#493=FACE_OUTER_BOUND('',#660,.T.);
#494=FACE_OUTER_BOUND('',#661,.T.);
#495=FACE_OUTER_BOUND('',#662,.T.);
#496=FACE_OUTER_BOUND('',#664,.T.);
#497=FACE_OUTER_BOUND('',#665,.T.);
#498=FACE_OUTER_BOUND('',#667,.T.);
#499=FACE_OUTER_BOUND('',#668,.T.);
#500=FACE_OUTER_BOUND('',#669,.T.);
#501=FACE_OUTER_BOUND('',#670,.T.);
#502=FACE_OUTER_BOUND('',#671,.T.);
#503=FACE_OUTER_BOUND('',#672,.T.);
#504=FACE_OUTER_BOUND('',#674,.T.);
#505=FACE_OUTER_BOUND('',#676,.T.);
#506=FACE_OUTER_BOUND('',#677,.T.);
#507=FACE_OUTER_BOUND('',#679,.T.);
#508=FACE_OUTER_BOUND('',#681,.T.);
#509=FACE_OUTER_BOUND('',#682,.T.);
#510=FACE_OUTER_BOUND('',#684,.T.);
#511=FACE_OUTER_BOUND('',#685,.T.);
#512=FACE_OUTER_BOUND('',#686,.T.);
#513=FACE_OUTER_BOUND('',#687,.T.);
#514=FACE_OUTER_BOUND('',#688,.T.);
#515=FACE_OUTER_BOUND('',#689,.T.);
#516=FACE_OUTER_BOUND('',#690,.T.);
#517=FACE_OUTER_BOUND('',#692,.T.);
#518=FACE_OUTER_BOUND('',#694,.T.);
#519=FACE_OUTER_BOUND('',#695,.T.);
#520=FACE_OUTER_BOUND('',#696,.T.);
#521=FACE_OUTER_BOUND('',#697,.T.);
#522=FACE_OUTER_BOUND('',#698,.T.);
#523=FACE_OUTER_BOUND('',#699,.T.);
#524=FACE_OUTER_BOUND('',#700,.T.);
#525=FACE_OUTER_BOUND('',#701,.T.);
#526=FACE_OUTER_BOUND('',#703,.T.);
#527=FACE_OUTER_BOUND('',#705,.T.);
#528=FACE_OUTER_BOUND('',#706,.T.);
#529=FACE_OUTER_BOUND('',#708,.T.);
#530=FACE_OUTER_BOUND('',#709,.T.);
#531=FACE_OUTER_BOUND('',#710,.T.);
#532=FACE_OUTER_BOUND('',#711,.T.);
#533=FACE_OUTER_BOUND('',#712,.T.);
#534=FACE_OUTER_BOUND('',#713,.T.);
#535=FACE_OUTER_BOUND('',#714,.T.);
#536=FACE_OUTER_BOUND('',#716,.T.);
#537=FACE_OUTER_BOUND('',#718,.T.);
#538=FACE_OUTER_BOUND('',#719,.T.);
#539=FACE_OUTER_BOUND('',#720,.T.);
#540=FACE_OUTER_BOUND('',#722,.T.);
#541=EDGE_LOOP('',(#1485,#1486,#1487,#1488));
#542=EDGE_LOOP('',(#1489,#1490,#1491,#1492));
#543=EDGE_LOOP('',(#1493,#1494,#1495,#1496));
#544=EDGE_LOOP('',(#1497,#1498,#1499,#1500));
#545=EDGE_LOOP('',(#1501,#1502,#1503,#1504));
#546=EDGE_LOOP('',(#1505,#1506,#1507,#1508));
#547=EDGE_LOOP('',(#1509,#1510,#1511,#1512));
#548=EDGE_LOOP('',(#1513,#1514,#1515,#1516));
#549=EDGE_LOOP('',(#1517,#1518,#1519,#1520));
#550=EDGE_LOOP('',(#1521));
#551=EDGE_LOOP('',(#1522));
#552=EDGE_LOOP('',(#1523));
#553=EDGE_LOOP('',(#1524));
#554=EDGE_LOOP('',(#1525,#1526,#1527,#1528));
#555=EDGE_LOOP('',(#1529));
#556=EDGE_LOOP('',(#1530));
#557=EDGE_LOOP('',(#1531));
#558=EDGE_LOOP('',(#1532));
#559=EDGE_LOOP('',(#1533,#1534,#1535,#1536));
#560=EDGE_LOOP('',(#1537,#1538,#1539,#1540));
#561=EDGE_LOOP('',(#1541,#1542,#1543,#1544));
#562=EDGE_LOOP('',(#1545,#1546,#1547,#1548));
#563=EDGE_LOOP('',(#1549,#1550,#1551,#1552));
#564=EDGE_LOOP('',(#1553,#1554,#1555,#1556));
#565=EDGE_LOOP('',(#1557,#1558,#1559,#1560));
#566=EDGE_LOOP('',(#1561,#1562,#1563,#1564));
#567=EDGE_LOOP('',(#1565,#1566,#1567,#1568));
#568=EDGE_LOOP('',(#1569,#1570,#1571,#1572,#1573,#1574));
#569=EDGE_LOOP('',(#1575));
#570=EDGE_LOOP('',(#1576));
#571=EDGE_LOOP('',(#1577));
#572=EDGE_LOOP('',(#1578,#1579,#1580,#1581,#1582,#1583));
#573=EDGE_LOOP('',(#1584));
#574=EDGE_LOOP('',(#1585));
#575=EDGE_LOOP('',(#1586));
#576=EDGE_LOOP('',(#1587,#1588,#1589,#1590));
#577=EDGE_LOOP('',(#1591,#1592,#1593,#1594));
#578=EDGE_LOOP('',(#1595,#1596,#1597,#1598));
#579=EDGE_LOOP('',(#1599,#1600,#1601,#1602));
#580=EDGE_LOOP('',(#1603,#1604,#1605,#1606));
#581=EDGE_LOOP('',(#1607,#1608,#1609,#1610));
#582=EDGE_LOOP('',(#1611,#1612,#1613,#1614));
#583=EDGE_LOOP('',(#1615));
#584=EDGE_LOOP('',(#1616));
#585=EDGE_LOOP('',(#1617,#1618,#1619,#1620));
#586=EDGE_LOOP('',(#1621));
#587=EDGE_LOOP('',(#1622));
#588=EDGE_LOOP('',(#1623,#1624,#1625,#1626));
#589=EDGE_LOOP('',(#1627,#1628,#1629,#1630));
#590=EDGE_LOOP('',(#1631,#1632,#1633,#1634));
#591=EDGE_LOOP('',(#1635,#1636,#1637,#1638));
#592=EDGE_LOOP('',(#1639,#1640,#1641,#1642));
#593=EDGE_LOOP('',(#1643,#1644,#1645,#1646));
#594=EDGE_LOOP('',(#1647,#1648,#1649,#1650));
#595=EDGE_LOOP('',(#1651));
#596=EDGE_LOOP('',(#1652));
#597=EDGE_LOOP('',(#1653,#1654,#1655,#1656));
#598=EDGE_LOOP('',(#1657));
#599=EDGE_LOOP('',(#1658));
#600=EDGE_LOOP('',(#1659,#1660,#1661,#1662));
#601=EDGE_LOOP('',(#1663,#1664,#1665,#1666));
#602=EDGE_LOOP('',(#1667,#1668,#1669,#1670));
#603=EDGE_LOOP('',(#1671,#1672,#1673,#1674));
#604=EDGE_LOOP('',(#1675,#1676,#1677,#1678));
#605=EDGE_LOOP('',(#1679,#1680,#1681,#1682));
#606=EDGE_LOOP('',(#1683,#1684,#1685,#1686));
#607=EDGE_LOOP('',(#1687,#1688,#1689,#1690));
#608=EDGE_LOOP('',(#1691));
#609=EDGE_LOOP('',(#1692));
#610=EDGE_LOOP('',(#1693));
#611=EDGE_LOOP('',(#1694,#1695,#1696,#1697));
#612=EDGE_LOOP('',(#1698));
#613=EDGE_LOOP('',(#1699));
#614=EDGE_LOOP('',(#1700));
#615=EDGE_LOOP('',(#1701,#1702,#1703,#1704));
#616=EDGE_LOOP('',(#1705,#1706,#1707,#1708));
#617=EDGE_LOOP('',(#1709,#1710,#1711,#1712));
#618=EDGE_LOOP('',(#1713,#1714,#1715,#1716));
#619=EDGE_LOOP('',(#1717,#1718,#1719,#1720));
#620=EDGE_LOOP('',(#1721,#1722,#1723,#1724));
#621=EDGE_LOOP('',(#1725,#1726,#1727,#1728));
#622=EDGE_LOOP('',(#1729));
#623=EDGE_LOOP('',(#1730));
#624=EDGE_LOOP('',(#1731,#1732,#1733,#1734));
#625=EDGE_LOOP('',(#1735));
#626=EDGE_LOOP('',(#1736));
#627=EDGE_LOOP('',(#1737,#1738,#1739,#1740));
#628=EDGE_LOOP('',(#1741,#1742,#1743,#1744));
#629=EDGE_LOOP('',(#1745,#1746,#1747,#1748));
#630=EDGE_LOOP('',(#1749,#1750,#1751,#1752));
#631=EDGE_LOOP('',(#1753,#1754,#1755,#1756));
#632=EDGE_LOOP('',(#1757,#1758,#1759,#1760));
#633=EDGE_LOOP('',(#1761,#1762,#1763,#1764));
#634=EDGE_LOOP('',(#1765));
#635=EDGE_LOOP('',(#1766));
#636=EDGE_LOOP('',(#1767,#1768,#1769,#1770));
#637=EDGE_LOOP('',(#1771));
#638=EDGE_LOOP('',(#1772));
#639=EDGE_LOOP('',(#1773,#1774,#1775,#1776));
#640=EDGE_LOOP('',(#1777));
#641=EDGE_LOOP('',(#1778));
#642=EDGE_LOOP('',(#1779,#1780,#1781,#1782));
#643=EDGE_LOOP('',(#1783,#1784,#1785,#1786));
#644=EDGE_LOOP('',(#1787));
#645=EDGE_LOOP('',(#1788));
#646=EDGE_LOOP('',(#1789));
#647=EDGE_LOOP('',(#1790));
#648=EDGE_LOOP('',(#1791,#1792,#1793,#1794));
#649=EDGE_LOOP('',(#1795));
#650=EDGE_LOOP('',(#1796));
#651=EDGE_LOOP('',(#1797));
#652=EDGE_LOOP('',(#1798));
#653=EDGE_LOOP('',(#1799,#1800,#1801,#1802));
#654=EDGE_LOOP('',(#1803));
#655=EDGE_LOOP('',(#1804));
#656=EDGE_LOOP('',(#1805,#1806,#1807,#1808));
#657=EDGE_LOOP('',(#1809));
#658=EDGE_LOOP('',(#1810,#1811,#1812,#1813));
#659=EDGE_LOOP('',(#1814));
#660=EDGE_LOOP('',(#1815,#1816,#1817,#1818));
#661=EDGE_LOOP('',(#1819,#1820,#1821,#1822));
#662=EDGE_LOOP('',(#1823));
#663=EDGE_LOOP('',(#1824));
#664=EDGE_LOOP('',(#1825,#1826,#1827,#1828));
#665=EDGE_LOOP('',(#1829));
#666=EDGE_LOOP('',(#1830));
#667=EDGE_LOOP('',(#1831,#1832,#1833,#1834));
#668=EDGE_LOOP('',(#1835,#1836,#1837,#1838));
#669=EDGE_LOOP('',(#1839,#1840,#1841,#1842));
#670=EDGE_LOOP('',(#1843,#1844,#1845,#1846));
#671=EDGE_LOOP('',(#1847,#1848,#1849,#1850));
#672=EDGE_LOOP('',(#1851));
#673=EDGE_LOOP('',(#1852));
#674=EDGE_LOOP('',(#1853));
#675=EDGE_LOOP('',(#1854));
#676=EDGE_LOOP('',(#1855,#1856,#1857,#1858));
#677=EDGE_LOOP('',(#1859));
#678=EDGE_LOOP('',(#1860));
#679=EDGE_LOOP('',(#1861));
#680=EDGE_LOOP('',(#1862));
#681=EDGE_LOOP('',(#1863,#1864,#1865,#1866));
#682=EDGE_LOOP('',(#1867));
#683=EDGE_LOOP('',(#1868));
#684=EDGE_LOOP('',(#1869,#1870,#1871,#1872));
#685=EDGE_LOOP('',(#1873));
#686=EDGE_LOOP('',(#1874,#1875,#1876,#1877));
#687=EDGE_LOOP('',(#1878));
#688=EDGE_LOOP('',(#1879,#1880,#1881,#1882));
#689=EDGE_LOOP('',(#1883,#1884,#1885,#1886));
#690=EDGE_LOOP('',(#1887));
#691=EDGE_LOOP('',(#1888));
#692=EDGE_LOOP('',(#1889));
#693=EDGE_LOOP('',(#1890));
#694=EDGE_LOOP('',(#1891,#1892,#1893,#1894));
#695=EDGE_LOOP('',(#1895,#1896,#1897,#1898));
#696=EDGE_LOOP('',(#1899,#1900,#1901,#1902));
#697=EDGE_LOOP('',(#1903,#1904,#1905,#1906));
#698=EDGE_LOOP('',(#1907,#1908,#1909,#1910));
#699=EDGE_LOOP('',(#1911,#1912,#1913,#1914));
#700=EDGE_LOOP('',(#1915,#1916,#1917,#1918));
#701=EDGE_LOOP('',(#1919));
#702=EDGE_LOOP('',(#1920));
#703=EDGE_LOOP('',(#1921));
#704=EDGE_LOOP('',(#1922));
#705=EDGE_LOOP('',(#1923,#1924,#1925,#1926));
#706=EDGE_LOOP('',(#1927));
#707=EDGE_LOOP('',(#1928));
#708=EDGE_LOOP('',(#1929,#1930,#1931,#1932));
#709=EDGE_LOOP('',(#1933));
#710=EDGE_LOOP('',(#1934,#1935,#1936,#1937));
#711=EDGE_LOOP('',(#1938));
#712=EDGE_LOOP('',(#1939,#1940,#1941,#1942));
#713=EDGE_LOOP('',(#1943,#1944,#1945,#1946));
#714=EDGE_LOOP('',(#1947));
#715=EDGE_LOOP('',(#1948));
#716=EDGE_LOOP('',(#1949));
#717=EDGE_LOOP('',(#1950));
#718=EDGE_LOOP('',(#1951,#1952,#1953,#1954));
#719=EDGE_LOOP('',(#1955,#1956,#1957,#1958));
#720=EDGE_LOOP('',(#1959));
#721=EDGE_LOOP('',(#1960));
#722=EDGE_LOOP('',(#1961));
#723=EDGE_LOOP('',(#1962));
#724=LINE('',#3422,#849);
#725=LINE('',#3428,#850);
#726=LINE('',#3434,#851);
#727=LINE('',#3440,#852);
#728=LINE('',#3445,#853);
#729=LINE('',#3447,#854);
#730=LINE('',#3449,#855);
#731=LINE('',#3450,#856);
#732=LINE('',#3453,#857);
#733=LINE('',#3455,#858);
#734=LINE('',#3456,#859);
#735=LINE('',#3459,#860);
#736=LINE('',#3461,#861);
#737=LINE('',#3462,#862);
#738=LINE('',#3464,#863);
#739=LINE('',#3465,#864);
#740=LINE('',#3473,#865);
#741=LINE('',#3479,#866);
#742=LINE('',#3485,#867);
#743=LINE('',#3490,#868);
#744=LINE('',#3492,#869);
#745=LINE('',#3494,#870);
#746=LINE('',#3495,#871);
#747=LINE('',#3498,#872);
#748=LINE('',#3500,#873);
#749=LINE('',#3501,#874);
#750=LINE('',#3504,#875);
#751=LINE('',#3506,#876);
#752=LINE('',#3507,#877);
#753=LINE('',#3511,#878);
#754=LINE('',#3513,#879);
#755=LINE('',#3515,#880);
#756=LINE('',#3516,#881);
#757=LINE('',#3518,#882);
#758=LINE('',#3519,#883);
#759=LINE('',#3521,#884);
#760=LINE('',#3522,#885);
#761=LINE('',#3530,#886);
#762=LINE('',#3536,#887);
#763=LINE('',#3541,#888);
#764=LINE('',#3543,#889);
#765=LINE('',#3545,#890);
#766=LINE('',#3546,#891);
#767=LINE('',#3552,#892);
#768=LINE('',#3555,#893);
#769=LINE('',#3557,#894);
#770=LINE('',#3558,#895);
#771=LINE('',#3569,#896);
#772=LINE('',#3575,#897);
#773=LINE('',#3580,#898);
#774=LINE('',#3582,#899);
#775=LINE('',#3584,#900);
#776=LINE('',#3585,#901);
#777=LINE('',#3591,#902);
#778=LINE('',#3594,#903);
#779=LINE('',#3596,#904);
#780=LINE('',#3597,#905);
#781=LINE('',#3608,#906);
#782=LINE('',#3614,#907);
#783=LINE('',#3620,#908);
#784=LINE('',#3625,#909);
#785=LINE('',#3627,#910);
#786=LINE('',#3629,#911);
#787=LINE('',#3630,#912);
#788=LINE('',#3636,#913);
#789=LINE('',#3639,#914);
#790=LINE('',#3641,#915);
#791=LINE('',#3642,#916);
#792=LINE('',#3653,#917);
#793=LINE('',#3659,#918);
#794=LINE('',#3664,#919);
#795=LINE('',#3666,#920);
#796=LINE('',#3668,#921);
#797=LINE('',#3669,#922);
#798=LINE('',#3675,#923);
#799=LINE('',#3678,#924);
#800=LINE('',#3680,#925);
#801=LINE('',#3681,#926);
#802=LINE('',#3692,#927);
#803=LINE('',#3698,#928);
#804=LINE('',#3703,#929);
#805=LINE('',#3705,#930);
#806=LINE('',#3707,#931);
#807=LINE('',#3708,#932);
#808=LINE('',#3714,#933);
#809=LINE('',#3717,#934);
#810=LINE('',#3719,#935);
#811=LINE('',#3720,#936);
#812=LINE('',#3731,#937);
#813=LINE('',#3740,#938);
#814=LINE('',#3746,#939);
#815=LINE('',#3755,#940);
#816=LINE('',#3766,#941);
#817=LINE('',#3774,#942);
#818=LINE('',#3778,#943);
#819=LINE('',#3785,#944);
#820=LINE('',#3790,#945);
#821=LINE('',#3797,#946);
#822=LINE('',#3804,#947);
#823=LINE('',#3808,#948);
#824=LINE('',#3810,#949);
#825=LINE('',#3816,#950);
#826=LINE('',#3822,#951);
#827=LINE('',#3831,#952);
#828=LINE('',#3842,#953);
#829=LINE('',#3850,#954);
#830=LINE('',#3854,#955);
#831=LINE('',#3861,#956);
#832=LINE('',#3867,#957);
#833=LINE('',#3875,#958);
#834=LINE('',#3877,#959);
#835=LINE('',#3879,#960);
#836=LINE('',#3880,#961);
#837=LINE('',#3884,#962);
#838=LINE('',#3886,#963);
#839=LINE('',#3888,#964);
#840=LINE('',#3889,#965);
#841=LINE('',#3903,#966);
#842=LINE('',#3914,#967);
#843=LINE('',#3922,#968);
#844=LINE('',#3926,#969);
#845=LINE('',#3933,#970);
#846=LINE('',#3939,#971);
#847=LINE('',#3948,#972);
#848=LINE('',#3954,#973);
#849=VECTOR('',#2679,4.5);
#850=VECTOR('',#2686,4.5);
#851=VECTOR('',#2693,4.5);
#852=VECTOR('',#2700,4.5);
#853=VECTOR('',#2705,10.);
#854=VECTOR('',#2706,10.);
#855=VECTOR('',#2707,10.);
#856=VECTOR('',#2708,10.);
#857=VECTOR('',#2711,10.);
#858=VECTOR('',#2712,10.);
#859=VECTOR('',#2713,10.);
#860=VECTOR('',#2716,10.);
#861=VECTOR('',#2717,10.);
#862=VECTOR('',#2718,10.);
#863=VECTOR('',#2721,10.);
#864=VECTOR('',#2722,10.);
#865=VECTOR('',#2733,5.);
#866=VECTOR('',#2740,5.);
#867=VECTOR('',#2747,5.);
#868=VECTOR('',#2752,10.);
#869=VECTOR('',#2753,10.);
#870=VECTOR('',#2754,10.);
#871=VECTOR('',#2755,10.);
#872=VECTOR('',#2758,10.);
#873=VECTOR('',#2759,10.);
#874=VECTOR('',#2760,10.);
#875=VECTOR('',#2763,10.);
#876=VECTOR('',#2764,10.);
#877=VECTOR('',#2765,10.);
#878=VECTOR('',#2768,10.);
#879=VECTOR('',#2769,10.);
#880=VECTOR('',#2770,10.);
#881=VECTOR('',#2771,10.);
#882=VECTOR('',#2774,10.);
#883=VECTOR('',#2775,10.);
#884=VECTOR('',#2778,10.);
#885=VECTOR('',#2779,10.);
#886=VECTOR('',#2790,7.);
#887=VECTOR('',#2797,7.);
#888=VECTOR('',#2802,10.);
#889=VECTOR('',#2803,10.);
#890=VECTOR('',#2804,10.);
#891=VECTOR('',#2805,10.);
#892=VECTOR('',#2812,10.);
#893=VECTOR('',#2815,10.);
#894=VECTOR('',#2816,10.);
#895=VECTOR('',#2817,10.);
#896=VECTOR('',#2834,7.);
#897=VECTOR('',#2841,7.);
#898=VECTOR('',#2846,10.);
#899=VECTOR('',#2847,10.);
#900=VECTOR('',#2848,10.);
#901=VECTOR('',#2849,10.);
#902=VECTOR('',#2856,10.);
#903=VECTOR('',#2859,10.);
#904=VECTOR('',#2860,10.);
#905=VECTOR('',#2861,10.);
#906=VECTOR('',#2878,7.);
#907=VECTOR('',#2885,7.);
#908=VECTOR('',#2892,7.);
#909=VECTOR('',#2897,10.);
#910=VECTOR('',#2898,10.);
#911=VECTOR('',#2899,10.);
#912=VECTOR('',#2900,10.);
#913=VECTOR('',#2907,10.);
#914=VECTOR('',#2910,10.);
#915=VECTOR('',#2911,10.);
#916=VECTOR('',#2912,10.);
#917=VECTOR('',#2929,7.);
#918=VECTOR('',#2936,7.);
#919=VECTOR('',#2941,10.);
#920=VECTOR('',#2942,10.);
#921=VECTOR('',#2943,10.);
#922=VECTOR('',#2944,10.);
#923=VECTOR('',#2951,10.);
#924=VECTOR('',#2954,10.);
#925=VECTOR('',#2955,10.);
#926=VECTOR('',#2956,10.);
#927=VECTOR('',#2973,7.);
#928=VECTOR('',#2980,7.);
#929=VECTOR('',#2985,10.);
#930=VECTOR('',#2986,10.);
#931=VECTOR('',#2987,10.);
#932=VECTOR('',#2988,10.);
#933=VECTOR('',#2995,10.);
#934=VECTOR('',#2998,10.);
#935=VECTOR('',#2999,10.);
#936=VECTOR('',#3000,10.);
#937=VECTOR('',#3017,15.);
#938=VECTOR('',#3030,5.);
#939=VECTOR('',#3037,7.);
#940=VECTOR('',#3050,4.);
#941=VECTOR('',#3065,5.);
#942=VECTOR('',#3074,8.);
#943=VECTOR('',#3081,5.);
#944=VECTOR('',#3090,9.5);
#945=VECTOR('',#3097,10.);
#946=VECTOR('',#3106,9.5);
#947=VECTOR('',#3115,5.5);
#948=VECTOR('',#3120,5.);
#949=VECTOR('',#3123,5.5);
#950=VECTOR('',#3130,5.);
#951=VECTOR('',#3137,10.);
#952=VECTOR('',#3150,4.);
#953=VECTOR('',#3165,5.);
#954=VECTOR('',#3174,8.);
#955=VECTOR('',#3181,5.);
#956=VECTOR('',#3190,5.);
#957=VECTOR('',#3197,10.);
#958=VECTOR('',#3208,10.);
#959=VECTOR('',#3209,10.);
#960=VECTOR('',#3210,10.);
#961=VECTOR('',#3211,10.);
#962=VECTOR('',#3214,10.);
#963=VECTOR('',#3215,10.);
#964=VECTOR('',#3216,10.);
#965=VECTOR('',#3217,10.);
#966=VECTOR('',#3240,4.);
#967=VECTOR('',#3255,5.);
#968=VECTOR('',#3264,8.);
#969=VECTOR('',#3271,5.);
#970=VECTOR('',#3280,5.);
#971=VECTOR('',#3287,10.);
#972=VECTOR('',#3300,5.);
#973=VECTOR('',#3307,10.);
#974=CIRCLE('',#2364,4.5);
#975=CIRCLE('',#2365,4.5);
#976=CIRCLE('',#2367,4.5);
#977=CIRCLE('',#2368,4.5);
#978=CIRCLE('',#2370,4.5);
#979=CIRCLE('',#2371,4.5);
#980=CIRCLE('',#2373,4.5);
#981=CIRCLE('',#2374,4.5);
#982=CIRCLE('',#2383,5.);
#983=CIRCLE('',#2384,5.);
#984=CIRCLE('',#2386,5.);
#985=CIRCLE('',#2387,5.);
#986=CIRCLE('',#2389,5.);
#987=CIRCLE('',#2390,5.);
#988=CIRCLE('',#2401,7.);
#989=CIRCLE('',#2402,7.);
#990=CIRCLE('',#2404,7.);
#991=CIRCLE('',#2405,7.);
#992=CIRCLE('',#2408,12.);
#993=CIRCLE('',#2409,12.);
#994=CIRCLE('',#2412,12.);
#995=CIRCLE('',#2413,12.);
#996=CIRCLE('',#2418,7.);
#997=CIRCLE('',#2419,7.);
#998=CIRCLE('',#2421,7.);
#999=CIRCLE('',#2422,7.);
#1000=CIRCLE('',#2425,12.);
#1001=CIRCLE('',#2426,12.);
#1002=CIRCLE('',#2429,12.);
#1003=CIRCLE('',#2430,12.);
#1004=CIRCLE('',#2435,7.);
#1005=CIRCLE('',#2436,7.);
#1006=CIRCLE('',#2438,7.);
#1007=CIRCLE('',#2439,7.);
#1008=CIRCLE('',#2441,7.);
#1009=CIRCLE('',#2442,7.);
#1010=CIRCLE('',#2445,12.);
#1011=CIRCLE('',#2446,12.);
#1012=CIRCLE('',#2449,12.);
#1013=CIRCLE('',#2450,12.);
#1014=CIRCLE('',#2455,7.);
#1015=CIRCLE('',#2456,7.);
#1016=CIRCLE('',#2458,7.);
#1017=CIRCLE('',#2459,7.);
#1018=CIRCLE('',#2462,12.);
#1019=CIRCLE('',#2463,12.);
#1020=CIRCLE('',#2466,12.);
#1021=CIRCLE('',#2467,12.);
#1022=CIRCLE('',#2472,7.);
#1023=CIRCLE('',#2473,7.);
#1024=CIRCLE('',#2475,7.);
#1025=CIRCLE('',#2476,7.);
#1026=CIRCLE('',#2479,12.);
#1027=CIRCLE('',#2480,12.);
#1028=CIRCLE('',#2483,12.);
#1029=CIRCLE('',#2484,12.);
#1030=CIRCLE('',#2489,15.);
#1031=CIRCLE('',#2490,15.);
#1032=CIRCLE('',#2495,5.);
#1033=CIRCLE('',#2496,5.);
#1034=CIRCLE('',#2498,7.);
#1035=CIRCLE('',#2499,7.);
#1036=CIRCLE('',#2504,4.);
#1037=CIRCLE('',#2505,4.);
#1038=CIRCLE('',#2507,5.);
#1039=CIRCLE('',#2509,5.);
#1040=CIRCLE('',#2511,5.);
#1041=CIRCLE('',#2513,8.);
#1042=CIRCLE('',#2514,5.);
#1043=CIRCLE('',#2516,8.);
#1044=CIRCLE('',#2522,10.);
#1045=CIRCLE('',#2523,9.);
#1046=CIRCLE('',#2525,10.);
#1047=CIRCLE('',#2527,6.);
#1048=CIRCLE('',#2529,9.);
#1049=CIRCLE('',#2531,6.);
#1050=CIRCLE('',#2533,5.);
#1051=CIRCLE('',#2535,5.);
#1052=CIRCLE('',#2539,5.);
#1053=CIRCLE('',#2540,5.);
#1054=CIRCLE('',#2542,10.);
#1055=CIRCLE('',#2543,10.);
#1056=CIRCLE('',#2548,4.);
#1057=CIRCLE('',#2549,4.);
#1058=CIRCLE('',#2551,5.);
#1059=CIRCLE('',#2553,5.);
#1060=CIRCLE('',#2555,5.);
#1061=CIRCLE('',#2557,8.);
#1062=CIRCLE('',#2558,5.);
#1063=CIRCLE('',#2560,8.);
#1064=CIRCLE('',#2566,5.);
#1065=CIRCLE('',#2567,5.);
#1066=CIRCLE('',#2569,10.);
#1067=CIRCLE('',#2570,10.);
#1068=CIRCLE('',#2577,8.);
#1069=CIRCLE('',#2578,4.);
#1070=CIRCLE('',#2580,4.);
#1071=CIRCLE('',#2582,8.);
#1072=CIRCLE('',#2586,4.);
#1073=CIRCLE('',#2587,4.);
#1074=CIRCLE('',#2589,5.);
#1075=CIRCLE('',#2591,5.);
#1076=CIRCLE('',#2593,5.);
#1077=CIRCLE('',#2595,8.);
#1078=CIRCLE('',#2596,5.);
#1079=CIRCLE('',#2598,8.);
#1080=CIRCLE('',#2604,5.);
#1081=CIRCLE('',#2605,5.);
#1082=CIRCLE('',#2607,10.);
#1083=CIRCLE('',#2608,10.);
#1084=CIRCLE('',#2613,5.);
#1085=CIRCLE('',#2614,5.);
#1086=CIRCLE('',#2616,10.);
#1087=CIRCLE('',#2617,10.);
#1088=VERTEX_POINT('',#3419);
#1089=VERTEX_POINT('',#3421);
#1090=VERTEX_POINT('',#3425);
#1091=VERTEX_POINT('',#3427);
#1092=VERTEX_POINT('',#3431);
#1093=VERTEX_POINT('',#3433);
#1094=VERTEX_POINT('',#3437);
#1095=VERTEX_POINT('',#3439);
#1096=VERTEX_POINT('',#3443);
#1097=VERTEX_POINT('',#3444);
#1098=VERTEX_POINT('',#3446);
#1099=VERTEX_POINT('',#3448);
#1100=VERTEX_POINT('',#3452);
#1101=VERTEX_POINT('',#3454);
#1102=VERTEX_POINT('',#3458);
#1103=VERTEX_POINT('',#3460);
#1104=VERTEX_POINT('',#3470);
#1105=VERTEX_POINT('',#3472);
#1106=VERTEX_POINT('',#3476);
#1107=VERTEX_POINT('',#3478);
#1108=VERTEX_POINT('',#3482);
#1109=VERTEX_POINT('',#3484);
#1110=VERTEX_POINT('',#3488);
#1111=VERTEX_POINT('',#3489);
#1112=VERTEX_POINT('',#3491);
#1113=VERTEX_POINT('',#3493);
#1114=VERTEX_POINT('',#3497);
#1115=VERTEX_POINT('',#3499);
#1116=VERTEX_POINT('',#3503);
#1117=VERTEX_POINT('',#3505);
#1118=VERTEX_POINT('',#3509);
#1119=VERTEX_POINT('',#3510);
#1120=VERTEX_POINT('',#3512);
#1121=VERTEX_POINT('',#3514);
#1122=VERTEX_POINT('',#3527);
#1123=VERTEX_POINT('',#3529);
#1124=VERTEX_POINT('',#3533);
#1125=VERTEX_POINT('',#3535);
#1126=VERTEX_POINT('',#3539);
#1127=VERTEX_POINT('',#3540);
#1128=VERTEX_POINT('',#3542);
#1129=VERTEX_POINT('',#3544);
#1130=VERTEX_POINT('',#3548);
#1131=VERTEX_POINT('',#3550);
#1132=VERTEX_POINT('',#3554);
#1133=VERTEX_POINT('',#3556);
#1134=VERTEX_POINT('',#3566);
#1135=VERTEX_POINT('',#3568);
#1136=VERTEX_POINT('',#3572);
#1137=VERTEX_POINT('',#3574);
#1138=VERTEX_POINT('',#3578);
#1139=VERTEX_POINT('',#3579);
#1140=VERTEX_POINT('',#3581);
#1141=VERTEX_POINT('',#3583);
#1142=VERTEX_POINT('',#3587);
#1143=VERTEX_POINT('',#3589);
#1144=VERTEX_POINT('',#3593);
#1145=VERTEX_POINT('',#3595);
#1146=VERTEX_POINT('',#3605);
#1147=VERTEX_POINT('',#3607);
#1148=VERTEX_POINT('',#3611);
#1149=VERTEX_POINT('',#3613);
#1150=VERTEX_POINT('',#3617);
#1151=VERTEX_POINT('',#3619);
#1152=VERTEX_POINT('',#3623);
#1153=VERTEX_POINT('',#3624);
#1154=VERTEX_POINT('',#3626);
#1155=VERTEX_POINT('',#3628);
#1156=VERTEX_POINT('',#3632);
#1157=VERTEX_POINT('',#3634);
#1158=VERTEX_POINT('',#3638);
#1159=VERTEX_POINT('',#3640);
#1160=VERTEX_POINT('',#3650);
#1161=VERTEX_POINT('',#3652);
#1162=VERTEX_POINT('',#3656);
#1163=VERTEX_POINT('',#3658);
#1164=VERTEX_POINT('',#3662);
#1165=VERTEX_POINT('',#3663);
#1166=VERTEX_POINT('',#3665);
#1167=VERTEX_POINT('',#3667);
#1168=VERTEX_POINT('',#3671);
#1169=VERTEX_POINT('',#3673);
#1170=VERTEX_POINT('',#3677);
#1171=VERTEX_POINT('',#3679);
#1172=VERTEX_POINT('',#3689);
#1173=VERTEX_POINT('',#3691);
#1174=VERTEX_POINT('',#3695);
#1175=VERTEX_POINT('',#3697);
#1176=VERTEX_POINT('',#3701);
#1177=VERTEX_POINT('',#3702);
#1178=VERTEX_POINT('',#3704);
#1179=VERTEX_POINT('',#3706);
#1180=VERTEX_POINT('',#3710);
#1181=VERTEX_POINT('',#3712);
#1182=VERTEX_POINT('',#3716);
#1183=VERTEX_POINT('',#3718);
#1184=VERTEX_POINT('',#3728);
#1185=VERTEX_POINT('',#3730);
#1186=VERTEX_POINT('',#3737);
#1187=VERTEX_POINT('',#3739);
#1188=VERTEX_POINT('',#3743);
#1189=VERTEX_POINT('',#3745);
#1190=VERTEX_POINT('',#3752);
#1191=VERTEX_POINT('',#3754);
#1192=VERTEX_POINT('',#3758);
#1193=VERTEX_POINT('',#3761);
#1194=VERTEX_POINT('',#3764);
#1195=VERTEX_POINT('',#3768);
#1196=VERTEX_POINT('',#3770);
#1197=VERTEX_POINT('',#3773);
#1198=VERTEX_POINT('',#3782);
#1199=VERTEX_POINT('',#3784);
#1200=VERTEX_POINT('',#3788);
#1201=VERTEX_POINT('',#3792);
#1202=VERTEX_POINT('',#3795);
#1203=VERTEX_POINT('',#3799);
#1204=VERTEX_POINT('',#3802);
#1205=VERTEX_POINT('',#3806);
#1206=VERTEX_POINT('',#3813);
#1207=VERTEX_POINT('',#3815);
#1208=VERTEX_POINT('',#3819);
#1209=VERTEX_POINT('',#3821);
#1210=VERTEX_POINT('',#3828);
#1211=VERTEX_POINT('',#3830);
#1212=VERTEX_POINT('',#3834);
#1213=VERTEX_POINT('',#3837);
#1214=VERTEX_POINT('',#3840);
#1215=VERTEX_POINT('',#3844);
#1216=VERTEX_POINT('',#3846);
#1217=VERTEX_POINT('',#3849);
#1218=VERTEX_POINT('',#3858);
#1219=VERTEX_POINT('',#3860);
#1220=VERTEX_POINT('',#3864);
#1221=VERTEX_POINT('',#3866);
#1222=VERTEX_POINT('',#3873);
#1223=VERTEX_POINT('',#3874);
#1224=VERTEX_POINT('',#3876);
#1225=VERTEX_POINT('',#3878);
#1226=VERTEX_POINT('',#3882);
#1227=VERTEX_POINT('',#3883);
#1228=VERTEX_POINT('',#3885);
#1229=VERTEX_POINT('',#3887);
#1230=VERTEX_POINT('',#3900);
#1231=VERTEX_POINT('',#3902);
#1232=VERTEX_POINT('',#3906);
#1233=VERTEX_POINT('',#3909);
#1234=VERTEX_POINT('',#3912);
#1235=VERTEX_POINT('',#3916);
#1236=VERTEX_POINT('',#3918);
#1237=VERTEX_POINT('',#3921);
#1238=VERTEX_POINT('',#3930);
#1239=VERTEX_POINT('',#3932);
#1240=VERTEX_POINT('',#3936);
#1241=VERTEX_POINT('',#3938);
#1242=VERTEX_POINT('',#3945);
#1243=VERTEX_POINT('',#3947);
#1244=VERTEX_POINT('',#3951);
#1245=VERTEX_POINT('',#3953);
#1246=EDGE_CURVE('',#1088,#1088,#974,.T.);
#1247=EDGE_CURVE('',#1088,#1089,#724,.T.);
#1248=EDGE_CURVE('',#1089,#1089,#975,.T.);
#1249=EDGE_CURVE('',#1090,#1090,#976,.T.);
#1250=EDGE_CURVE('',#1090,#1091,#725,.T.);
#1251=EDGE_CURVE('',#1091,#1091,#977,.T.);
#1252=EDGE_CURVE('',#1092,#1092,#978,.T.);
#1253=EDGE_CURVE('',#1092,#1093,#726,.T.);
#1254=EDGE_CURVE('',#1093,#1093,#979,.T.);
#1255=EDGE_CURVE('',#1094,#1094,#980,.T.);
#1256=EDGE_CURVE('',#1094,#1095,#727,.T.);
#1257=EDGE_CURVE('',#1095,#1095,#981,.T.);
#1258=EDGE_CURVE('',#1096,#1097,#728,.F.);
#1259=EDGE_CURVE('',#1097,#1098,#729,.T.);
#1260=EDGE_CURVE('',#1099,#1098,#730,.F.);
#1261=EDGE_CURVE('',#1096,#1099,#731,.T.);
#1262=EDGE_CURVE('',#1100,#1096,#732,.F.);
#1263=EDGE_CURVE('',#1101,#1099,#733,.F.);
#1264=EDGE_CURVE('',#1100,#1101,#734,.T.);
#1265=EDGE_CURVE('',#1102,#1100,#735,.F.);
#1266=EDGE_CURVE('',#1103,#1101,#736,.F.);
#1267=EDGE_CURVE('',#1102,#1103,#737,.F.);
#1268=EDGE_CURVE('',#1097,#1102,#738,.F.);
#1269=EDGE_CURVE('',#1098,#1103,#739,.F.);
#1270=EDGE_CURVE('',#1104,#1104,#982,.T.);
#1271=EDGE_CURVE('',#1104,#1105,#740,.T.);
#1272=EDGE_CURVE('',#1105,#1105,#983,.T.);
#1273=EDGE_CURVE('',#1106,#1106,#984,.T.);
#1274=EDGE_CURVE('',#1106,#1107,#741,.T.);
#1275=EDGE_CURVE('',#1107,#1107,#985,.T.);
#1276=EDGE_CURVE('',#1108,#1108,#986,.T.);
#1277=EDGE_CURVE('',#1108,#1109,#742,.T.);
#1278=EDGE_CURVE('',#1109,#1109,#987,.T.);
#1279=EDGE_CURVE('',#1110,#1111,#743,.T.);
#1280=EDGE_CURVE('',#1112,#1111,#744,.T.);
#1281=EDGE_CURVE('',#1113,#1112,#745,.T.);
#1282=EDGE_CURVE('',#1110,#1113,#746,.T.);
#1283=EDGE_CURVE('',#1114,#1110,#747,.T.);
#1284=EDGE_CURVE('',#1115,#1113,#748,.T.);
#1285=EDGE_CURVE('',#1114,#1115,#749,.T.);
#1286=EDGE_CURVE('',#1111,#1116,#750,.T.);
#1287=EDGE_CURVE('',#1116,#1117,#751,.F.);
#1288=EDGE_CURVE('',#1112,#1117,#752,.T.);
#1289=EDGE_CURVE('',#1118,#1119,#753,.F.);
#1290=EDGE_CURVE('',#1119,#1120,#754,.F.);
#1291=EDGE_CURVE('',#1121,#1120,#755,.F.);
#1292=EDGE_CURVE('',#1118,#1121,#756,.F.);
#1293=EDGE_CURVE('',#1116,#1118,#757,.F.);
#1294=EDGE_CURVE('',#1117,#1121,#758,.F.);
#1295=EDGE_CURVE('',#1119,#1114,#759,.F.);
#1296=EDGE_CURVE('',#1120,#1115,#760,.F.);
#1297=EDGE_CURVE('',#1122,#1122,#988,.T.);
#1298=EDGE_CURVE('',#1122,#1123,#761,.T.);
#1299=EDGE_CURVE('',#1123,#1123,#989,.T.);
#1300=EDGE_CURVE('',#1124,#1124,#990,.T.);
#1301=EDGE_CURVE('',#1124,#1125,#762,.T.);
#1302=EDGE_CURVE('',#1125,#1125,#991,.T.);
#1303=EDGE_CURVE('',#1126,#1127,#763,.T.);
#1304=EDGE_CURVE('',#1127,#1128,#764,.T.);
#1305=EDGE_CURVE('',#1129,#1128,#765,.T.);
#1306=EDGE_CURVE('',#1126,#1129,#766,.T.);
#1307=EDGE_CURVE('',#1130,#1126,#992,.T.);
#1308=EDGE_CURVE('',#1131,#1129,#993,.T.);
#1309=EDGE_CURVE('',#1130,#1131,#767,.T.);
#1310=EDGE_CURVE('',#1132,#1130,#768,.T.);
#1311=EDGE_CURVE('',#1133,#1131,#769,.T.);
#1312=EDGE_CURVE('',#1132,#1133,#770,.T.);
#1313=EDGE_CURVE('',#1127,#1132,#994,.T.);
#1314=EDGE_CURVE('',#1128,#1133,#995,.T.);
#1315=EDGE_CURVE('',#1134,#1134,#996,.T.);
#1316=EDGE_CURVE('',#1134,#1135,#771,.T.);
#1317=EDGE_CURVE('',#1135,#1135,#997,.T.);
#1318=EDGE_CURVE('',#1136,#1136,#998,.T.);
#1319=EDGE_CURVE('',#1136,#1137,#772,.T.);
#1320=EDGE_CURVE('',#1137,#1137,#999,.T.);
#1321=EDGE_CURVE('',#1138,#1139,#773,.T.);
#1322=EDGE_CURVE('',#1139,#1140,#774,.T.);
#1323=EDGE_CURVE('',#1141,#1140,#775,.T.);
#1324=EDGE_CURVE('',#1138,#1141,#776,.T.);
#1325=EDGE_CURVE('',#1142,#1138,#1000,.T.);
#1326=EDGE_CURVE('',#1143,#1141,#1001,.T.);
#1327=EDGE_CURVE('',#1142,#1143,#777,.T.);
#1328=EDGE_CURVE('',#1144,#1142,#778,.T.);
#1329=EDGE_CURVE('',#1145,#1143,#779,.T.);
#1330=EDGE_CURVE('',#1144,#1145,#780,.T.);
#1331=EDGE_CURVE('',#1139,#1144,#1002,.T.);
#1332=EDGE_CURVE('',#1140,#1145,#1003,.T.);
#1333=EDGE_CURVE('',#1146,#1146,#1004,.T.);
#1334=EDGE_CURVE('',#1146,#1147,#781,.T.);
#1335=EDGE_CURVE('',#1147,#1147,#1005,.T.);
#1336=EDGE_CURVE('',#1148,#1148,#1006,.T.);
#1337=EDGE_CURVE('',#1148,#1149,#782,.T.);
#1338=EDGE_CURVE('',#1149,#1149,#1007,.T.);
#1339=EDGE_CURVE('',#1150,#1150,#1008,.T.);
#1340=EDGE_CURVE('',#1150,#1151,#783,.T.);
#1341=EDGE_CURVE('',#1151,#1151,#1009,.T.);
#1342=EDGE_CURVE('',#1152,#1153,#784,.T.);
#1343=EDGE_CURVE('',#1153,#1154,#785,.T.);
#1344=EDGE_CURVE('',#1155,#1154,#786,.T.);
#1345=EDGE_CURVE('',#1152,#1155,#787,.T.);
#1346=EDGE_CURVE('',#1156,#1152,#1010,.T.);
#1347=EDGE_CURVE('',#1157,#1155,#1011,.T.);
#1348=EDGE_CURVE('',#1156,#1157,#788,.T.);
#1349=EDGE_CURVE('',#1158,#1156,#789,.T.);
#1350=EDGE_CURVE('',#1159,#1157,#790,.T.);
#1351=EDGE_CURVE('',#1158,#1159,#791,.T.);
#1352=EDGE_CURVE('',#1153,#1158,#1012,.T.);
#1353=EDGE_CURVE('',#1154,#1159,#1013,.T.);
#1354=EDGE_CURVE('',#1160,#1160,#1014,.T.);
#1355=EDGE_CURVE('',#1160,#1161,#792,.T.);
#1356=EDGE_CURVE('',#1161,#1161,#1015,.T.);
#1357=EDGE_CURVE('',#1162,#1162,#1016,.T.);
#1358=EDGE_CURVE('',#1162,#1163,#793,.T.);
#1359=EDGE_CURVE('',#1163,#1163,#1017,.T.);
#1360=EDGE_CURVE('',#1164,#1165,#794,.T.);
#1361=EDGE_CURVE('',#1165,#1166,#795,.T.);
#1362=EDGE_CURVE('',#1167,#1166,#796,.T.);
#1363=EDGE_CURVE('',#1164,#1167,#797,.T.);
#1364=EDGE_CURVE('',#1168,#1164,#1018,.T.);
#1365=EDGE_CURVE('',#1169,#1167,#1019,.T.);
#1366=EDGE_CURVE('',#1168,#1169,#798,.T.);
#1367=EDGE_CURVE('',#1170,#1168,#799,.T.);
#1368=EDGE_CURVE('',#1171,#1169,#800,.T.);
#1369=EDGE_CURVE('',#1170,#1171,#801,.T.);
#1370=EDGE_CURVE('',#1165,#1170,#1020,.T.);
#1371=EDGE_CURVE('',#1166,#1171,#1021,.T.);
#1372=EDGE_CURVE('',#1172,#1172,#1022,.T.);
#1373=EDGE_CURVE('',#1172,#1173,#802,.T.);
#1374=EDGE_CURVE('',#1173,#1173,#1023,.T.);
#1375=EDGE_CURVE('',#1174,#1174,#1024,.T.);
#1376=EDGE_CURVE('',#1174,#1175,#803,.T.);
#1377=EDGE_CURVE('',#1175,#1175,#1025,.T.);
#1378=EDGE_CURVE('',#1176,#1177,#804,.T.);
#1379=EDGE_CURVE('',#1177,#1178,#805,.T.);
#1380=EDGE_CURVE('',#1179,#1178,#806,.T.);
#1381=EDGE_CURVE('',#1176,#1179,#807,.T.);
#1382=EDGE_CURVE('',#1180,#1176,#1026,.T.);
#1383=EDGE_CURVE('',#1181,#1179,#1027,.T.);
#1384=EDGE_CURVE('',#1180,#1181,#808,.T.);
#1385=EDGE_CURVE('',#1182,#1180,#809,.T.);
#1386=EDGE_CURVE('',#1183,#1181,#810,.T.);
#1387=EDGE_CURVE('',#1182,#1183,#811,.T.);
#1388=EDGE_CURVE('',#1177,#1182,#1028,.T.);
#1389=EDGE_CURVE('',#1178,#1183,#1029,.T.);
#1390=EDGE_CURVE('',#1184,#1184,#1030,.T.);
#1391=EDGE_CURVE('',#1184,#1185,#812,.T.);
#1392=EDGE_CURVE('',#1185,#1185,#1031,.T.);
#1393=EDGE_CURVE('',#1186,#1186,#1032,.T.);
#1394=EDGE_CURVE('',#1186,#1187,#813,.T.);
#1395=EDGE_CURVE('',#1187,#1187,#1033,.T.);
#1396=EDGE_CURVE('',#1188,#1188,#1034,.T.);
#1397=EDGE_CURVE('',#1188,#1189,#814,.T.);
#1398=EDGE_CURVE('',#1189,#1189,#1035,.T.);
#1399=EDGE_CURVE('',#1190,#1190,#1036,.T.);
#1400=EDGE_CURVE('',#1190,#1191,#815,.T.);
#1401=EDGE_CURVE('',#1191,#1191,#1037,.T.);
#1402=EDGE_CURVE('',#1192,#1192,#1038,.T.);
#1403=EDGE_CURVE('',#1193,#1193,#1039,.T.);
#1404=EDGE_CURVE('',#1194,#1194,#1040,.T.);
#1405=EDGE_CURVE('',#1194,#1193,#816,.T.);
#1406=EDGE_CURVE('',#1195,#1195,#1041,.T.);
#1407=EDGE_CURVE('',#1196,#1196,#1042,.T.);
#1408=EDGE_CURVE('',#1195,#1197,#817,.T.);
#1409=EDGE_CURVE('',#1197,#1197,#1043,.T.);
#1410=EDGE_CURVE('',#1192,#1196,#818,.T.);
#1411=EDGE_CURVE('',#1198,#1198,#1044,.T.);
#1412=EDGE_CURVE('',#1198,#1199,#819,.T.);
#1413=EDGE_CURVE('',#1199,#1199,#1045,.T.);
#1414=EDGE_CURVE('',#1200,#1200,#1046,.T.);
#1415=EDGE_CURVE('',#1200,#1198,#820,.T.);
#1416=EDGE_CURVE('',#1201,#1201,#1047,.T.);
#1417=EDGE_CURVE('',#1202,#1202,#1048,.T.);
#1418=EDGE_CURVE('',#1202,#1200,#821,.T.);
#1419=EDGE_CURVE('',#1203,#1203,#1049,.T.);
#1420=EDGE_CURVE('',#1204,#1204,#1050,.T.);
#1421=EDGE_CURVE('',#1204,#1201,#822,.T.);
#1422=EDGE_CURVE('',#1205,#1205,#1051,.T.);
#1423=EDGE_CURVE('',#1205,#1204,#823,.T.);
#1424=EDGE_CURVE('',#1203,#1205,#824,.T.);
#1425=EDGE_CURVE('',#1206,#1206,#1052,.T.);
#1426=EDGE_CURVE('',#1206,#1207,#825,.T.);
#1427=EDGE_CURVE('',#1207,#1207,#1053,.T.);
#1428=EDGE_CURVE('',#1208,#1208,#1054,.T.);
#1429=EDGE_CURVE('',#1208,#1209,#826,.T.);
#1430=EDGE_CURVE('',#1209,#1209,#1055,.T.);
#1431=EDGE_CURVE('',#1210,#1210,#1056,.T.);
#1432=EDGE_CURVE('',#1210,#1211,#827,.T.);
#1433=EDGE_CURVE('',#1211,#1211,#1057,.T.);
#1434=EDGE_CURVE('',#1212,#1212,#1058,.T.);
#1435=EDGE_CURVE('',#1213,#1213,#1059,.T.);
#1436=EDGE_CURVE('',#1214,#1214,#1060,.T.);
#1437=EDGE_CURVE('',#1214,#1213,#828,.T.);
#1438=EDGE_CURVE('',#1215,#1215,#1061,.T.);
#1439=EDGE_CURVE('',#1216,#1216,#1062,.T.);
#1440=EDGE_CURVE('',#1215,#1217,#829,.T.);
#1441=EDGE_CURVE('',#1217,#1217,#1063,.T.);
#1442=EDGE_CURVE('',#1212,#1216,#830,.T.);
#1443=EDGE_CURVE('',#1218,#1218,#1064,.T.);
#1444=EDGE_CURVE('',#1218,#1219,#831,.T.);
#1445=EDGE_CURVE('',#1219,#1219,#1065,.T.);
#1446=EDGE_CURVE('',#1220,#1220,#1066,.T.);
#1447=EDGE_CURVE('',#1220,#1221,#832,.T.);
#1448=EDGE_CURVE('',#1221,#1221,#1067,.T.);
#1449=EDGE_CURVE('',#1222,#1223,#833,.T.);
#1450=EDGE_CURVE('',#1224,#1222,#834,.T.);
#1451=EDGE_CURVE('',#1225,#1224,#835,.T.);
#1452=EDGE_CURVE('',#1223,#1225,#836,.T.);
#1453=EDGE_CURVE('',#1226,#1227,#837,.T.);
#1454=EDGE_CURVE('',#1228,#1226,#838,.T.);
#1455=EDGE_CURVE('',#1229,#1228,#839,.T.);
#1456=EDGE_CURVE('',#1227,#1229,#840,.T.);
#1457=EDGE_CURVE('',#1224,#1229,#1068,.T.);
#1458=EDGE_CURVE('',#1227,#1222,#1069,.T.);
#1459=EDGE_CURVE('',#1226,#1223,#1070,.T.);
#1460=EDGE_CURVE('',#1225,#1228,#1071,.T.);
#1461=EDGE_CURVE('',#1230,#1230,#1072,.T.);
#1462=EDGE_CURVE('',#1230,#1231,#841,.T.);
#1463=EDGE_CURVE('',#1231,#1231,#1073,.T.);
#1464=EDGE_CURVE('',#1232,#1232,#1074,.T.);
#1465=EDGE_CURVE('',#1233,#1233,#1075,.T.);
#1466=EDGE_CURVE('',#1234,#1234,#1076,.T.);
#1467=EDGE_CURVE('',#1234,#1233,#842,.T.);
#1468=EDGE_CURVE('',#1235,#1235,#1077,.T.);
#1469=EDGE_CURVE('',#1236,#1236,#1078,.T.);
#1470=EDGE_CURVE('',#1235,#1237,#843,.T.);
#1471=EDGE_CURVE('',#1237,#1237,#1079,.T.);
#1472=EDGE_CURVE('',#1232,#1236,#844,.T.);
#1473=EDGE_CURVE('',#1238,#1238,#1080,.T.);
#1474=EDGE_CURVE('',#1238,#1239,#845,.T.);
#1475=EDGE_CURVE('',#1239,#1239,#1081,.T.);
#1476=EDGE_CURVE('',#1240,#1240,#1082,.T.);
#1477=EDGE_CURVE('',#1240,#1241,#846,.T.);
#1478=EDGE_CURVE('',#1241,#1241,#1083,.T.);
#1479=EDGE_CURVE('',#1242,#1242,#1084,.T.);
#1480=EDGE_CURVE('',#1242,#1243,#847,.T.);
#1481=EDGE_CURVE('',#1243,#1243,#1085,.T.);
#1482=EDGE_CURVE('',#1244,#1244,#1086,.T.);
#1483=EDGE_CURVE('',#1244,#1245,#848,.T.);
#1484=EDGE_CURVE('',#1245,#1245,#1087,.T.);
#1485=ORIENTED_EDGE('',*,*,#1246,.F.);
#1486=ORIENTED_EDGE('',*,*,#1247,.T.);
#1487=ORIENTED_EDGE('',*,*,#1248,.F.);
#1488=ORIENTED_EDGE('',*,*,#1247,.F.);
#1489=ORIENTED_EDGE('',*,*,#1249,.F.);
#1490=ORIENTED_EDGE('',*,*,#1250,.T.);
#1491=ORIENTED_EDGE('',*,*,#1251,.F.);
#1492=ORIENTED_EDGE('',*,*,#1250,.F.);
#1493=ORIENTED_EDGE('',*,*,#1252,.F.);
#1494=ORIENTED_EDGE('',*,*,#1253,.T.);
#1495=ORIENTED_EDGE('',*,*,#1254,.F.);
#1496=ORIENTED_EDGE('',*,*,#1253,.F.);
#1497=ORIENTED_EDGE('',*,*,#1255,.F.);
#1498=ORIENTED_EDGE('',*,*,#1256,.T.);
#1499=ORIENTED_EDGE('',*,*,#1257,.F.);
#1500=ORIENTED_EDGE('',*,*,#1256,.F.);
#1501=ORIENTED_EDGE('',*,*,#1258,.T.);
#1502=ORIENTED_EDGE('',*,*,#1259,.T.);
#1503=ORIENTED_EDGE('',*,*,#1260,.F.);
#1504=ORIENTED_EDGE('',*,*,#1261,.F.);
#1505=ORIENTED_EDGE('',*,*,#1262,.T.);
#1506=ORIENTED_EDGE('',*,*,#1261,.T.);
#1507=ORIENTED_EDGE('',*,*,#1263,.F.);
#1508=ORIENTED_EDGE('',*,*,#1264,.F.);
#1509=ORIENTED_EDGE('',*,*,#1265,.T.);
#1510=ORIENTED_EDGE('',*,*,#1264,.T.);
#1511=ORIENTED_EDGE('',*,*,#1266,.F.);
#1512=ORIENTED_EDGE('',*,*,#1267,.F.);
#1513=ORIENTED_EDGE('',*,*,#1268,.T.);
#1514=ORIENTED_EDGE('',*,*,#1267,.T.);
#1515=ORIENTED_EDGE('',*,*,#1269,.F.);
#1516=ORIENTED_EDGE('',*,*,#1259,.F.);
#1517=ORIENTED_EDGE('',*,*,#1269,.T.);
#1518=ORIENTED_EDGE('',*,*,#1266,.T.);
#1519=ORIENTED_EDGE('',*,*,#1263,.T.);
#1520=ORIENTED_EDGE('',*,*,#1260,.T.);
#1521=ORIENTED_EDGE('',*,*,#1246,.T.);
#1522=ORIENTED_EDGE('',*,*,#1249,.T.);
#1523=ORIENTED_EDGE('',*,*,#1252,.T.);
#1524=ORIENTED_EDGE('',*,*,#1255,.T.);
#1525=ORIENTED_EDGE('',*,*,#1268,.F.);
#1526=ORIENTED_EDGE('',*,*,#1258,.F.);
#1527=ORIENTED_EDGE('',*,*,#1262,.F.);
#1528=ORIENTED_EDGE('',*,*,#1265,.F.);
#1529=ORIENTED_EDGE('',*,*,#1248,.T.);
#1530=ORIENTED_EDGE('',*,*,#1251,.T.);
#1531=ORIENTED_EDGE('',*,*,#1254,.T.);
#1532=ORIENTED_EDGE('',*,*,#1257,.T.);
#1533=ORIENTED_EDGE('',*,*,#1270,.F.);
#1534=ORIENTED_EDGE('',*,*,#1271,.T.);
#1535=ORIENTED_EDGE('',*,*,#1272,.F.);
#1536=ORIENTED_EDGE('',*,*,#1271,.F.);
#1537=ORIENTED_EDGE('',*,*,#1273,.F.);
#1538=ORIENTED_EDGE('',*,*,#1274,.T.);
#1539=ORIENTED_EDGE('',*,*,#1275,.F.);
#1540=ORIENTED_EDGE('',*,*,#1274,.F.);
#1541=ORIENTED_EDGE('',*,*,#1276,.F.);
#1542=ORIENTED_EDGE('',*,*,#1277,.T.);
#1543=ORIENTED_EDGE('',*,*,#1278,.F.);
#1544=ORIENTED_EDGE('',*,*,#1277,.F.);
#1545=ORIENTED_EDGE('',*,*,#1279,.T.);
#1546=ORIENTED_EDGE('',*,*,#1280,.F.);
#1547=ORIENTED_EDGE('',*,*,#1281,.F.);
#1548=ORIENTED_EDGE('',*,*,#1282,.F.);
#1549=ORIENTED_EDGE('',*,*,#1283,.T.);
#1550=ORIENTED_EDGE('',*,*,#1282,.T.);
#1551=ORIENTED_EDGE('',*,*,#1284,.F.);
#1552=ORIENTED_EDGE('',*,*,#1285,.F.);
#1553=ORIENTED_EDGE('',*,*,#1280,.T.);
#1554=ORIENTED_EDGE('',*,*,#1286,.T.);
#1555=ORIENTED_EDGE('',*,*,#1287,.T.);
#1556=ORIENTED_EDGE('',*,*,#1288,.F.);
#1557=ORIENTED_EDGE('',*,*,#1289,.T.);
#1558=ORIENTED_EDGE('',*,*,#1290,.T.);
#1559=ORIENTED_EDGE('',*,*,#1291,.F.);
#1560=ORIENTED_EDGE('',*,*,#1292,.F.);
#1561=ORIENTED_EDGE('',*,*,#1293,.T.);
#1562=ORIENTED_EDGE('',*,*,#1292,.T.);
#1563=ORIENTED_EDGE('',*,*,#1294,.F.);
#1564=ORIENTED_EDGE('',*,*,#1287,.F.);
#1565=ORIENTED_EDGE('',*,*,#1295,.T.);
#1566=ORIENTED_EDGE('',*,*,#1285,.T.);
#1567=ORIENTED_EDGE('',*,*,#1296,.F.);
#1568=ORIENTED_EDGE('',*,*,#1290,.F.);
#1569=ORIENTED_EDGE('',*,*,#1296,.T.);
#1570=ORIENTED_EDGE('',*,*,#1284,.T.);
#1571=ORIENTED_EDGE('',*,*,#1281,.T.);
#1572=ORIENTED_EDGE('',*,*,#1288,.T.);
#1573=ORIENTED_EDGE('',*,*,#1294,.T.);
#1574=ORIENTED_EDGE('',*,*,#1291,.T.);
#1575=ORIENTED_EDGE('',*,*,#1270,.T.);
#1576=ORIENTED_EDGE('',*,*,#1273,.T.);
#1577=ORIENTED_EDGE('',*,*,#1276,.T.);
#1578=ORIENTED_EDGE('',*,*,#1295,.F.);
#1579=ORIENTED_EDGE('',*,*,#1289,.F.);
#1580=ORIENTED_EDGE('',*,*,#1293,.F.);
#1581=ORIENTED_EDGE('',*,*,#1286,.F.);
#1582=ORIENTED_EDGE('',*,*,#1279,.F.);
#1583=ORIENTED_EDGE('',*,*,#1283,.F.);
#1584=ORIENTED_EDGE('',*,*,#1272,.T.);
#1585=ORIENTED_EDGE('',*,*,#1275,.T.);
#1586=ORIENTED_EDGE('',*,*,#1278,.T.);
#1587=ORIENTED_EDGE('',*,*,#1297,.F.);
#1588=ORIENTED_EDGE('',*,*,#1298,.T.);
#1589=ORIENTED_EDGE('',*,*,#1299,.F.);
#1590=ORIENTED_EDGE('',*,*,#1298,.F.);
#1591=ORIENTED_EDGE('',*,*,#1300,.F.);
#1592=ORIENTED_EDGE('',*,*,#1301,.T.);
#1593=ORIENTED_EDGE('',*,*,#1302,.F.);
#1594=ORIENTED_EDGE('',*,*,#1301,.F.);
#1595=ORIENTED_EDGE('',*,*,#1303,.T.);
#1596=ORIENTED_EDGE('',*,*,#1304,.T.);
#1597=ORIENTED_EDGE('',*,*,#1305,.F.);
#1598=ORIENTED_EDGE('',*,*,#1306,.F.);
#1599=ORIENTED_EDGE('',*,*,#1307,.T.);
#1600=ORIENTED_EDGE('',*,*,#1306,.T.);
#1601=ORIENTED_EDGE('',*,*,#1308,.F.);
#1602=ORIENTED_EDGE('',*,*,#1309,.F.);
#1603=ORIENTED_EDGE('',*,*,#1310,.T.);
#1604=ORIENTED_EDGE('',*,*,#1309,.T.);
#1605=ORIENTED_EDGE('',*,*,#1311,.F.);
#1606=ORIENTED_EDGE('',*,*,#1312,.F.);
#1607=ORIENTED_EDGE('',*,*,#1313,.T.);
#1608=ORIENTED_EDGE('',*,*,#1312,.T.);
#1609=ORIENTED_EDGE('',*,*,#1314,.F.);
#1610=ORIENTED_EDGE('',*,*,#1304,.F.);
#1611=ORIENTED_EDGE('',*,*,#1314,.T.);
#1612=ORIENTED_EDGE('',*,*,#1311,.T.);
#1613=ORIENTED_EDGE('',*,*,#1308,.T.);
#1614=ORIENTED_EDGE('',*,*,#1305,.T.);
#1615=ORIENTED_EDGE('',*,*,#1297,.T.);
#1616=ORIENTED_EDGE('',*,*,#1300,.T.);
#1617=ORIENTED_EDGE('',*,*,#1313,.F.);
#1618=ORIENTED_EDGE('',*,*,#1303,.F.);
#1619=ORIENTED_EDGE('',*,*,#1307,.F.);
#1620=ORIENTED_EDGE('',*,*,#1310,.F.);
#1621=ORIENTED_EDGE('',*,*,#1299,.T.);
#1622=ORIENTED_EDGE('',*,*,#1302,.T.);
#1623=ORIENTED_EDGE('',*,*,#1315,.F.);
#1624=ORIENTED_EDGE('',*,*,#1316,.T.);
#1625=ORIENTED_EDGE('',*,*,#1317,.F.);
#1626=ORIENTED_EDGE('',*,*,#1316,.F.);
#1627=ORIENTED_EDGE('',*,*,#1318,.F.);
#1628=ORIENTED_EDGE('',*,*,#1319,.T.);
#1629=ORIENTED_EDGE('',*,*,#1320,.F.);
#1630=ORIENTED_EDGE('',*,*,#1319,.F.);
#1631=ORIENTED_EDGE('',*,*,#1321,.T.);
#1632=ORIENTED_EDGE('',*,*,#1322,.T.);
#1633=ORIENTED_EDGE('',*,*,#1323,.F.);
#1634=ORIENTED_EDGE('',*,*,#1324,.F.);
#1635=ORIENTED_EDGE('',*,*,#1325,.T.);
#1636=ORIENTED_EDGE('',*,*,#1324,.T.);
#1637=ORIENTED_EDGE('',*,*,#1326,.F.);
#1638=ORIENTED_EDGE('',*,*,#1327,.F.);
#1639=ORIENTED_EDGE('',*,*,#1328,.T.);
#1640=ORIENTED_EDGE('',*,*,#1327,.T.);
#1641=ORIENTED_EDGE('',*,*,#1329,.F.);
#1642=ORIENTED_EDGE('',*,*,#1330,.F.);
#1643=ORIENTED_EDGE('',*,*,#1331,.T.);
#1644=ORIENTED_EDGE('',*,*,#1330,.T.);
#1645=ORIENTED_EDGE('',*,*,#1332,.F.);
#1646=ORIENTED_EDGE('',*,*,#1322,.F.);
#1647=ORIENTED_EDGE('',*,*,#1332,.T.);
#1648=ORIENTED_EDGE('',*,*,#1329,.T.);
#1649=ORIENTED_EDGE('',*,*,#1326,.T.);
#1650=ORIENTED_EDGE('',*,*,#1323,.T.);
#1651=ORIENTED_EDGE('',*,*,#1315,.T.);
#1652=ORIENTED_EDGE('',*,*,#1318,.T.);
#1653=ORIENTED_EDGE('',*,*,#1331,.F.);
#1654=ORIENTED_EDGE('',*,*,#1321,.F.);
#1655=ORIENTED_EDGE('',*,*,#1325,.F.);
#1656=ORIENTED_EDGE('',*,*,#1328,.F.);
#1657=ORIENTED_EDGE('',*,*,#1317,.T.);
#1658=ORIENTED_EDGE('',*,*,#1320,.T.);
#1659=ORIENTED_EDGE('',*,*,#1333,.F.);
#1660=ORIENTED_EDGE('',*,*,#1334,.T.);
#1661=ORIENTED_EDGE('',*,*,#1335,.F.);
#1662=ORIENTED_EDGE('',*,*,#1334,.F.);
#1663=ORIENTED_EDGE('',*,*,#1336,.F.);
#1664=ORIENTED_EDGE('',*,*,#1337,.T.);
#1665=ORIENTED_EDGE('',*,*,#1338,.F.);
#1666=ORIENTED_EDGE('',*,*,#1337,.F.);
#1667=ORIENTED_EDGE('',*,*,#1339,.F.);
#1668=ORIENTED_EDGE('',*,*,#1340,.T.);
#1669=ORIENTED_EDGE('',*,*,#1341,.F.);
#1670=ORIENTED_EDGE('',*,*,#1340,.F.);
#1671=ORIENTED_EDGE('',*,*,#1342,.T.);
#1672=ORIENTED_EDGE('',*,*,#1343,.T.);
#1673=ORIENTED_EDGE('',*,*,#1344,.F.);
#1674=ORIENTED_EDGE('',*,*,#1345,.F.);
#1675=ORIENTED_EDGE('',*,*,#1346,.T.);
#1676=ORIENTED_EDGE('',*,*,#1345,.T.);
#1677=ORIENTED_EDGE('',*,*,#1347,.F.);
#1678=ORIENTED_EDGE('',*,*,#1348,.F.);
#1679=ORIENTED_EDGE('',*,*,#1349,.T.);
#1680=ORIENTED_EDGE('',*,*,#1348,.T.);
#1681=ORIENTED_EDGE('',*,*,#1350,.F.);
#1682=ORIENTED_EDGE('',*,*,#1351,.F.);
#1683=ORIENTED_EDGE('',*,*,#1352,.T.);
#1684=ORIENTED_EDGE('',*,*,#1351,.T.);
#1685=ORIENTED_EDGE('',*,*,#1353,.F.);
#1686=ORIENTED_EDGE('',*,*,#1343,.F.);
#1687=ORIENTED_EDGE('',*,*,#1353,.T.);
#1688=ORIENTED_EDGE('',*,*,#1350,.T.);
#1689=ORIENTED_EDGE('',*,*,#1347,.T.);
#1690=ORIENTED_EDGE('',*,*,#1344,.T.);
#1691=ORIENTED_EDGE('',*,*,#1333,.T.);
#1692=ORIENTED_EDGE('',*,*,#1336,.T.);
#1693=ORIENTED_EDGE('',*,*,#1339,.T.);
#1694=ORIENTED_EDGE('',*,*,#1352,.F.);
#1695=ORIENTED_EDGE('',*,*,#1342,.F.);
#1696=ORIENTED_EDGE('',*,*,#1346,.F.);
#1697=ORIENTED_EDGE('',*,*,#1349,.F.);
#1698=ORIENTED_EDGE('',*,*,#1335,.T.);
#1699=ORIENTED_EDGE('',*,*,#1338,.T.);
#1700=ORIENTED_EDGE('',*,*,#1341,.T.);
#1701=ORIENTED_EDGE('',*,*,#1354,.F.);
#1702=ORIENTED_EDGE('',*,*,#1355,.T.);
#1703=ORIENTED_EDGE('',*,*,#1356,.F.);
#1704=ORIENTED_EDGE('',*,*,#1355,.F.);
#1705=ORIENTED_EDGE('',*,*,#1357,.F.);
#1706=ORIENTED_EDGE('',*,*,#1358,.T.);
#1707=ORIENTED_EDGE('',*,*,#1359,.F.);
#1708=ORIENTED_EDGE('',*,*,#1358,.F.);
#1709=ORIENTED_EDGE('',*,*,#1360,.T.);
#1710=ORIENTED_EDGE('',*,*,#1361,.T.);
#1711=ORIENTED_EDGE('',*,*,#1362,.F.);
#1712=ORIENTED_EDGE('',*,*,#1363,.F.);
#1713=ORIENTED_EDGE('',*,*,#1364,.T.);
#1714=ORIENTED_EDGE('',*,*,#1363,.T.);
#1715=ORIENTED_EDGE('',*,*,#1365,.F.);
#1716=ORIENTED_EDGE('',*,*,#1366,.F.);
#1717=ORIENTED_EDGE('',*,*,#1367,.T.);
#1718=ORIENTED_EDGE('',*,*,#1366,.T.);
#1719=ORIENTED_EDGE('',*,*,#1368,.F.);
#1720=ORIENTED_EDGE('',*,*,#1369,.F.);
#1721=ORIENTED_EDGE('',*,*,#1370,.T.);
#1722=ORIENTED_EDGE('',*,*,#1369,.T.);
#1723=ORIENTED_EDGE('',*,*,#1371,.F.);
#1724=ORIENTED_EDGE('',*,*,#1361,.F.);
#1725=ORIENTED_EDGE('',*,*,#1371,.T.);
#1726=ORIENTED_EDGE('',*,*,#1368,.T.);
#1727=ORIENTED_EDGE('',*,*,#1365,.T.);
#1728=ORIENTED_EDGE('',*,*,#1362,.T.);
#1729=ORIENTED_EDGE('',*,*,#1354,.T.);
#1730=ORIENTED_EDGE('',*,*,#1357,.T.);
#1731=ORIENTED_EDGE('',*,*,#1370,.F.);
#1732=ORIENTED_EDGE('',*,*,#1360,.F.);
#1733=ORIENTED_EDGE('',*,*,#1364,.F.);
#1734=ORIENTED_EDGE('',*,*,#1367,.F.);
#1735=ORIENTED_EDGE('',*,*,#1356,.T.);
#1736=ORIENTED_EDGE('',*,*,#1359,.T.);
#1737=ORIENTED_EDGE('',*,*,#1372,.F.);
#1738=ORIENTED_EDGE('',*,*,#1373,.T.);
#1739=ORIENTED_EDGE('',*,*,#1374,.F.);
#1740=ORIENTED_EDGE('',*,*,#1373,.F.);
#1741=ORIENTED_EDGE('',*,*,#1375,.F.);
#1742=ORIENTED_EDGE('',*,*,#1376,.T.);
#1743=ORIENTED_EDGE('',*,*,#1377,.F.);
#1744=ORIENTED_EDGE('',*,*,#1376,.F.);
#1745=ORIENTED_EDGE('',*,*,#1378,.T.);
#1746=ORIENTED_EDGE('',*,*,#1379,.T.);
#1747=ORIENTED_EDGE('',*,*,#1380,.F.);
#1748=ORIENTED_EDGE('',*,*,#1381,.F.);
#1749=ORIENTED_EDGE('',*,*,#1382,.T.);
#1750=ORIENTED_EDGE('',*,*,#1381,.T.);
#1751=ORIENTED_EDGE('',*,*,#1383,.F.);
#1752=ORIENTED_EDGE('',*,*,#1384,.F.);
#1753=ORIENTED_EDGE('',*,*,#1385,.T.);
#1754=ORIENTED_EDGE('',*,*,#1384,.T.);
#1755=ORIENTED_EDGE('',*,*,#1386,.F.);
#1756=ORIENTED_EDGE('',*,*,#1387,.F.);
#1757=ORIENTED_EDGE('',*,*,#1388,.T.);
#1758=ORIENTED_EDGE('',*,*,#1387,.T.);
#1759=ORIENTED_EDGE('',*,*,#1389,.F.);
#1760=ORIENTED_EDGE('',*,*,#1379,.F.);
#1761=ORIENTED_EDGE('',*,*,#1389,.T.);
#1762=ORIENTED_EDGE('',*,*,#1386,.T.);
#1763=ORIENTED_EDGE('',*,*,#1383,.T.);
#1764=ORIENTED_EDGE('',*,*,#1380,.T.);
#1765=ORIENTED_EDGE('',*,*,#1372,.T.);
#1766=ORIENTED_EDGE('',*,*,#1375,.T.);
#1767=ORIENTED_EDGE('',*,*,#1388,.F.);
#1768=ORIENTED_EDGE('',*,*,#1378,.F.);
#1769=ORIENTED_EDGE('',*,*,#1382,.F.);
#1770=ORIENTED_EDGE('',*,*,#1385,.F.);
#1771=ORIENTED_EDGE('',*,*,#1374,.T.);
#1772=ORIENTED_EDGE('',*,*,#1377,.T.);
#1773=ORIENTED_EDGE('',*,*,#1390,.F.);
#1774=ORIENTED_EDGE('',*,*,#1391,.T.);
#1775=ORIENTED_EDGE('',*,*,#1392,.T.);
#1776=ORIENTED_EDGE('',*,*,#1391,.F.);
#1777=ORIENTED_EDGE('',*,*,#1390,.T.);
#1778=ORIENTED_EDGE('',*,*,#1392,.F.);
#1779=ORIENTED_EDGE('',*,*,#1393,.F.);
#1780=ORIENTED_EDGE('',*,*,#1394,.T.);
#1781=ORIENTED_EDGE('',*,*,#1395,.T.);
#1782=ORIENTED_EDGE('',*,*,#1394,.F.);
#1783=ORIENTED_EDGE('',*,*,#1396,.F.);
#1784=ORIENTED_EDGE('',*,*,#1397,.T.);
#1785=ORIENTED_EDGE('',*,*,#1398,.T.);
#1786=ORIENTED_EDGE('',*,*,#1397,.F.);
#1787=ORIENTED_EDGE('',*,*,#1396,.T.);
#1788=ORIENTED_EDGE('',*,*,#1393,.T.);
#1789=ORIENTED_EDGE('',*,*,#1398,.F.);
#1790=ORIENTED_EDGE('',*,*,#1395,.F.);
#1791=ORIENTED_EDGE('',*,*,#1399,.T.);
#1792=ORIENTED_EDGE('',*,*,#1400,.T.);
#1793=ORIENTED_EDGE('',*,*,#1401,.F.);
#1794=ORIENTED_EDGE('',*,*,#1400,.F.);
#1795=ORIENTED_EDGE('',*,*,#1402,.F.);
#1796=ORIENTED_EDGE('',*,*,#1399,.F.);
#1797=ORIENTED_EDGE('',*,*,#1403,.F.);
#1798=ORIENTED_EDGE('',*,*,#1401,.T.);
#1799=ORIENTED_EDGE('',*,*,#1404,.F.);
#1800=ORIENTED_EDGE('',*,*,#1405,.T.);
#1801=ORIENTED_EDGE('',*,*,#1403,.T.);
#1802=ORIENTED_EDGE('',*,*,#1405,.F.);
#1803=ORIENTED_EDGE('',*,*,#1406,.T.);
#1804=ORIENTED_EDGE('',*,*,#1407,.F.);
#1805=ORIENTED_EDGE('',*,*,#1406,.F.);
#1806=ORIENTED_EDGE('',*,*,#1408,.T.);
#1807=ORIENTED_EDGE('',*,*,#1409,.T.);
#1808=ORIENTED_EDGE('',*,*,#1408,.F.);
#1809=ORIENTED_EDGE('',*,*,#1409,.F.);
#1810=ORIENTED_EDGE('',*,*,#1402,.T.);
#1811=ORIENTED_EDGE('',*,*,#1410,.T.);
#1812=ORIENTED_EDGE('',*,*,#1407,.T.);
#1813=ORIENTED_EDGE('',*,*,#1410,.F.);
#1814=ORIENTED_EDGE('',*,*,#1404,.T.);
#1815=ORIENTED_EDGE('',*,*,#1411,.T.);
#1816=ORIENTED_EDGE('',*,*,#1412,.T.);
#1817=ORIENTED_EDGE('',*,*,#1413,.T.);
#1818=ORIENTED_EDGE('',*,*,#1412,.F.);
#1819=ORIENTED_EDGE('',*,*,#1414,.F.);
#1820=ORIENTED_EDGE('',*,*,#1415,.T.);
#1821=ORIENTED_EDGE('',*,*,#1411,.F.);
#1822=ORIENTED_EDGE('',*,*,#1415,.F.);
#1823=ORIENTED_EDGE('',*,*,#1413,.F.);
#1824=ORIENTED_EDGE('',*,*,#1416,.F.);
#1825=ORIENTED_EDGE('',*,*,#1417,.T.);
#1826=ORIENTED_EDGE('',*,*,#1418,.T.);
#1827=ORIENTED_EDGE('',*,*,#1414,.T.);
#1828=ORIENTED_EDGE('',*,*,#1418,.F.);
#1829=ORIENTED_EDGE('',*,*,#1417,.F.);
#1830=ORIENTED_EDGE('',*,*,#1419,.F.);
#1831=ORIENTED_EDGE('',*,*,#1420,.T.);
#1832=ORIENTED_EDGE('',*,*,#1421,.T.);
#1833=ORIENTED_EDGE('',*,*,#1416,.T.);
#1834=ORIENTED_EDGE('',*,*,#1421,.F.);
#1835=ORIENTED_EDGE('',*,*,#1422,.F.);
#1836=ORIENTED_EDGE('',*,*,#1423,.T.);
#1837=ORIENTED_EDGE('',*,*,#1420,.F.);
#1838=ORIENTED_EDGE('',*,*,#1423,.F.);
#1839=ORIENTED_EDGE('',*,*,#1419,.T.);
#1840=ORIENTED_EDGE('',*,*,#1424,.T.);
#1841=ORIENTED_EDGE('',*,*,#1422,.T.);
#1842=ORIENTED_EDGE('',*,*,#1424,.F.);
#1843=ORIENTED_EDGE('',*,*,#1425,.F.);
#1844=ORIENTED_EDGE('',*,*,#1426,.T.);
#1845=ORIENTED_EDGE('',*,*,#1427,.T.);
#1846=ORIENTED_EDGE('',*,*,#1426,.F.);
#1847=ORIENTED_EDGE('',*,*,#1428,.F.);
#1848=ORIENTED_EDGE('',*,*,#1429,.T.);
#1849=ORIENTED_EDGE('',*,*,#1430,.T.);
#1850=ORIENTED_EDGE('',*,*,#1429,.F.);
#1851=ORIENTED_EDGE('',*,*,#1428,.T.);
#1852=ORIENTED_EDGE('',*,*,#1425,.T.);
#1853=ORIENTED_EDGE('',*,*,#1430,.F.);
#1854=ORIENTED_EDGE('',*,*,#1427,.F.);
#1855=ORIENTED_EDGE('',*,*,#1431,.T.);
#1856=ORIENTED_EDGE('',*,*,#1432,.T.);
#1857=ORIENTED_EDGE('',*,*,#1433,.F.);
#1858=ORIENTED_EDGE('',*,*,#1432,.F.);
#1859=ORIENTED_EDGE('',*,*,#1434,.F.);
#1860=ORIENTED_EDGE('',*,*,#1431,.F.);
#1861=ORIENTED_EDGE('',*,*,#1435,.F.);
#1862=ORIENTED_EDGE('',*,*,#1433,.T.);
#1863=ORIENTED_EDGE('',*,*,#1436,.F.);
#1864=ORIENTED_EDGE('',*,*,#1437,.T.);
#1865=ORIENTED_EDGE('',*,*,#1435,.T.);
#1866=ORIENTED_EDGE('',*,*,#1437,.F.);
#1867=ORIENTED_EDGE('',*,*,#1438,.T.);
#1868=ORIENTED_EDGE('',*,*,#1439,.F.);
#1869=ORIENTED_EDGE('',*,*,#1438,.F.);
#1870=ORIENTED_EDGE('',*,*,#1440,.T.);
#1871=ORIENTED_EDGE('',*,*,#1441,.T.);
#1872=ORIENTED_EDGE('',*,*,#1440,.F.);
#1873=ORIENTED_EDGE('',*,*,#1441,.F.);
#1874=ORIENTED_EDGE('',*,*,#1434,.T.);
#1875=ORIENTED_EDGE('',*,*,#1442,.T.);
#1876=ORIENTED_EDGE('',*,*,#1439,.T.);
#1877=ORIENTED_EDGE('',*,*,#1442,.F.);
#1878=ORIENTED_EDGE('',*,*,#1436,.T.);
#1879=ORIENTED_EDGE('',*,*,#1443,.F.);
#1880=ORIENTED_EDGE('',*,*,#1444,.T.);
#1881=ORIENTED_EDGE('',*,*,#1445,.T.);
#1882=ORIENTED_EDGE('',*,*,#1444,.F.);
#1883=ORIENTED_EDGE('',*,*,#1446,.F.);
#1884=ORIENTED_EDGE('',*,*,#1447,.T.);
#1885=ORIENTED_EDGE('',*,*,#1448,.T.);
#1886=ORIENTED_EDGE('',*,*,#1447,.F.);
#1887=ORIENTED_EDGE('',*,*,#1446,.T.);
#1888=ORIENTED_EDGE('',*,*,#1443,.T.);
#1889=ORIENTED_EDGE('',*,*,#1448,.F.);
#1890=ORIENTED_EDGE('',*,*,#1445,.F.);
#1891=ORIENTED_EDGE('',*,*,#1449,.F.);
#1892=ORIENTED_EDGE('',*,*,#1450,.F.);
#1893=ORIENTED_EDGE('',*,*,#1451,.F.);
#1894=ORIENTED_EDGE('',*,*,#1452,.F.);
#1895=ORIENTED_EDGE('',*,*,#1453,.F.);
#1896=ORIENTED_EDGE('',*,*,#1454,.F.);
#1897=ORIENTED_EDGE('',*,*,#1455,.F.);
#1898=ORIENTED_EDGE('',*,*,#1456,.F.);
#1899=ORIENTED_EDGE('',*,*,#1456,.T.);
#1900=ORIENTED_EDGE('',*,*,#1457,.F.);
#1901=ORIENTED_EDGE('',*,*,#1450,.T.);
#1902=ORIENTED_EDGE('',*,*,#1458,.F.);
#1903=ORIENTED_EDGE('',*,*,#1453,.T.);
#1904=ORIENTED_EDGE('',*,*,#1458,.T.);
#1905=ORIENTED_EDGE('',*,*,#1449,.T.);
#1906=ORIENTED_EDGE('',*,*,#1459,.F.);
#1907=ORIENTED_EDGE('',*,*,#1455,.T.);
#1908=ORIENTED_EDGE('',*,*,#1460,.F.);
#1909=ORIENTED_EDGE('',*,*,#1451,.T.);
#1910=ORIENTED_EDGE('',*,*,#1457,.T.);
#1911=ORIENTED_EDGE('',*,*,#1454,.T.);
#1912=ORIENTED_EDGE('',*,*,#1459,.T.);
#1913=ORIENTED_EDGE('',*,*,#1452,.T.);
#1914=ORIENTED_EDGE('',*,*,#1460,.T.);
#1915=ORIENTED_EDGE('',*,*,#1461,.T.);
#1916=ORIENTED_EDGE('',*,*,#1462,.T.);
#1917=ORIENTED_EDGE('',*,*,#1463,.F.);
#1918=ORIENTED_EDGE('',*,*,#1462,.F.);
#1919=ORIENTED_EDGE('',*,*,#1464,.F.);
#1920=ORIENTED_EDGE('',*,*,#1461,.F.);
#1921=ORIENTED_EDGE('',*,*,#1465,.F.);
#1922=ORIENTED_EDGE('',*,*,#1463,.T.);
#1923=ORIENTED_EDGE('',*,*,#1466,.F.);
#1924=ORIENTED_EDGE('',*,*,#1467,.T.);
#1925=ORIENTED_EDGE('',*,*,#1465,.T.);
#1926=ORIENTED_EDGE('',*,*,#1467,.F.);
#1927=ORIENTED_EDGE('',*,*,#1468,.T.);
#1928=ORIENTED_EDGE('',*,*,#1469,.F.);
#1929=ORIENTED_EDGE('',*,*,#1468,.F.);
#1930=ORIENTED_EDGE('',*,*,#1470,.T.);
#1931=ORIENTED_EDGE('',*,*,#1471,.T.);
#1932=ORIENTED_EDGE('',*,*,#1470,.F.);
#1933=ORIENTED_EDGE('',*,*,#1471,.F.);
#1934=ORIENTED_EDGE('',*,*,#1464,.T.);
#1935=ORIENTED_EDGE('',*,*,#1472,.T.);
#1936=ORIENTED_EDGE('',*,*,#1469,.T.);
#1937=ORIENTED_EDGE('',*,*,#1472,.F.);
#1938=ORIENTED_EDGE('',*,*,#1466,.T.);
#1939=ORIENTED_EDGE('',*,*,#1473,.F.);
#1940=ORIENTED_EDGE('',*,*,#1474,.T.);
#1941=ORIENTED_EDGE('',*,*,#1475,.T.);
#1942=ORIENTED_EDGE('',*,*,#1474,.F.);
#1943=ORIENTED_EDGE('',*,*,#1476,.F.);
#1944=ORIENTED_EDGE('',*,*,#1477,.T.);
#1945=ORIENTED_EDGE('',*,*,#1478,.T.);
#1946=ORIENTED_EDGE('',*,*,#1477,.F.);
#1947=ORIENTED_EDGE('',*,*,#1476,.T.);
#1948=ORIENTED_EDGE('',*,*,#1473,.T.);
#1949=ORIENTED_EDGE('',*,*,#1478,.F.);
#1950=ORIENTED_EDGE('',*,*,#1475,.F.);
#1951=ORIENTED_EDGE('',*,*,#1479,.F.);
#1952=ORIENTED_EDGE('',*,*,#1480,.T.);
#1953=ORIENTED_EDGE('',*,*,#1481,.T.);
#1954=ORIENTED_EDGE('',*,*,#1480,.F.);
#1955=ORIENTED_EDGE('',*,*,#1482,.F.);
#1956=ORIENTED_EDGE('',*,*,#1483,.T.);
#1957=ORIENTED_EDGE('',*,*,#1484,.T.);
#1958=ORIENTED_EDGE('',*,*,#1483,.F.);
#1959=ORIENTED_EDGE('',*,*,#1482,.T.);
#1960=ORIENTED_EDGE('',*,*,#1479,.T.);
#1961=ORIENTED_EDGE('',*,*,#1484,.F.);
#1962=ORIENTED_EDGE('',*,*,#1481,.F.);
#1963=CYLINDRICAL_SURFACE('',#2363,4.5);
#1964=CYLINDRICAL_SURFACE('',#2366,4.5);
#1965=CYLINDRICAL_SURFACE('',#2369,4.5);
#1966=CYLINDRICAL_SURFACE('',#2372,4.5);
#1967=CYLINDRICAL_SURFACE('',#2382,5.);
#1968=CYLINDRICAL_SURFACE('',#2385,5.);
#1969=CYLINDRICAL_SURFACE('',#2388,5.);
#1970=CYLINDRICAL_SURFACE('',#2400,7.);
#1971=CYLINDRICAL_SURFACE('',#2403,7.);
#1972=CYLINDRICAL_SURFACE('',#2407,12.);
#1973=CYLINDRICAL_SURFACE('',#2411,12.);
#1974=CYLINDRICAL_SURFACE('',#2417,7.);
#1975=CYLINDRICAL_SURFACE('',#2420,7.);
#1976=CYLINDRICAL_SURFACE('',#2424,12.);
#1977=CYLINDRICAL_SURFACE('',#2428,12.);
#1978=CYLINDRICAL_SURFACE('',#2434,7.);
#1979=CYLINDRICAL_SURFACE('',#2437,7.);
#1980=CYLINDRICAL_SURFACE('',#2440,7.);
#1981=CYLINDRICAL_SURFACE('',#2444,12.);
#1982=CYLINDRICAL_SURFACE('',#2448,12.);
#1983=CYLINDRICAL_SURFACE('',#2454,7.);
#1984=CYLINDRICAL_SURFACE('',#2457,7.);
#1985=CYLINDRICAL_SURFACE('',#2461,12.);
#1986=CYLINDRICAL_SURFACE('',#2465,12.);
#1987=CYLINDRICAL_SURFACE('',#2471,7.);
#1988=CYLINDRICAL_SURFACE('',#2474,7.);
#1989=CYLINDRICAL_SURFACE('',#2478,12.);
#1990=CYLINDRICAL_SURFACE('',#2482,12.);
#1991=CYLINDRICAL_SURFACE('',#2488,15.);
#1992=CYLINDRICAL_SURFACE('',#2494,5.);
#1993=CYLINDRICAL_SURFACE('',#2497,7.);
#1994=CYLINDRICAL_SURFACE('',#2503,4.);
#1995=CYLINDRICAL_SURFACE('',#2510,5.);
#1996=CYLINDRICAL_SURFACE('',#2515,8.);
#1997=CYLINDRICAL_SURFACE('',#2518,5.);
#1998=CYLINDRICAL_SURFACE('',#2524,10.);
#1999=CYLINDRICAL_SURFACE('',#2534,5.);
#2000=CYLINDRICAL_SURFACE('',#2538,5.);
#2001=CYLINDRICAL_SURFACE('',#2541,10.);
#2002=CYLINDRICAL_SURFACE('',#2547,4.);
#2003=CYLINDRICAL_SURFACE('',#2554,5.);
#2004=CYLINDRICAL_SURFACE('',#2559,8.);
#2005=CYLINDRICAL_SURFACE('',#2562,5.);
#2006=CYLINDRICAL_SURFACE('',#2565,5.);
#2007=CYLINDRICAL_SURFACE('',#2568,10.);
#2008=CYLINDRICAL_SURFACE('',#2579,4.);
#2009=CYLINDRICAL_SURFACE('',#2581,8.);
#2010=CYLINDRICAL_SURFACE('',#2585,4.);
#2011=CYLINDRICAL_SURFACE('',#2592,5.);
#2012=CYLINDRICAL_SURFACE('',#2597,8.);
#2013=CYLINDRICAL_SURFACE('',#2600,5.);
#2014=CYLINDRICAL_SURFACE('',#2603,5.);
#2015=CYLINDRICAL_SURFACE('',#2606,10.);
#2016=CYLINDRICAL_SURFACE('',#2612,5.);
#2017=CYLINDRICAL_SURFACE('',#2615,10.);
#2018=ADVANCED_FACE('',(#415),#1963,.F.);
#2019=ADVANCED_FACE('',(#416),#1964,.F.);
#2020=ADVANCED_FACE('',(#417),#1965,.F.);
#2021=ADVANCED_FACE('',(#418),#1966,.F.);
#2022=ADVANCED_FACE('',(#419),#348,.T.);
#2023=ADVANCED_FACE('',(#420),#349,.T.);
#2024=ADVANCED_FACE('',(#421),#350,.T.);
#2025=ADVANCED_FACE('',(#422),#351,.T.);
#2026=ADVANCED_FACE('',(#423,#291,#292,#293,#294),#352,.T.);
#2027=ADVANCED_FACE('',(#424,#295,#296,#297,#298),#353,.F.);
#2028=ADVANCED_FACE('',(#425),#1967,.F.);
#2029=ADVANCED_FACE('',(#426),#1968,.F.);
#2030=ADVANCED_FACE('',(#427),#1969,.F.);
#2031=ADVANCED_FACE('',(#428),#354,.T.);
#2032=ADVANCED_FACE('',(#429),#355,.T.);
#2033=ADVANCED_FACE('',(#430),#356,.T.);
#2034=ADVANCED_FACE('',(#431),#357,.T.);
#2035=ADVANCED_FACE('',(#432),#358,.T.);
#2036=ADVANCED_FACE('',(#433),#359,.T.);
#2037=ADVANCED_FACE('',(#434,#299,#300,#301),#360,.T.);
#2038=ADVANCED_FACE('',(#435,#302,#303,#304),#361,.F.);
#2039=ADVANCED_FACE('',(#436),#1970,.F.);
#2040=ADVANCED_FACE('',(#437),#1971,.F.);
#2041=ADVANCED_FACE('',(#438),#362,.T.);
#2042=ADVANCED_FACE('',(#439),#1972,.T.);
#2043=ADVANCED_FACE('',(#440),#363,.T.);
#2044=ADVANCED_FACE('',(#441),#1973,.T.);
#2045=ADVANCED_FACE('',(#442,#305,#306),#364,.T.);
#2046=ADVANCED_FACE('',(#443,#307,#308),#365,.F.);
#2047=ADVANCED_FACE('',(#444),#1974,.F.);
#2048=ADVANCED_FACE('',(#445),#1975,.F.);
#2049=ADVANCED_FACE('',(#446),#366,.T.);
#2050=ADVANCED_FACE('',(#447),#1976,.T.);
#2051=ADVANCED_FACE('',(#448),#367,.T.);
#2052=ADVANCED_FACE('',(#449),#1977,.T.);
#2053=ADVANCED_FACE('',(#450,#309,#310),#368,.T.);
#2054=ADVANCED_FACE('',(#451,#311,#312),#369,.F.);
#2055=ADVANCED_FACE('',(#452),#1978,.F.);
#2056=ADVANCED_FACE('',(#453),#1979,.F.);
#2057=ADVANCED_FACE('',(#454),#1980,.F.);
#2058=ADVANCED_FACE('',(#455),#370,.T.);
#2059=ADVANCED_FACE('',(#456),#1981,.T.);
#2060=ADVANCED_FACE('',(#457),#371,.T.);
#2061=ADVANCED_FACE('',(#458),#1982,.T.);
#2062=ADVANCED_FACE('',(#459,#313,#314,#315),#372,.T.);
#2063=ADVANCED_FACE('',(#460,#316,#317,#318),#373,.F.);
#2064=ADVANCED_FACE('',(#461),#1983,.F.);
#2065=ADVANCED_FACE('',(#462),#1984,.F.);
#2066=ADVANCED_FACE('',(#463),#374,.T.);
#2067=ADVANCED_FACE('',(#464),#1985,.T.);
#2068=ADVANCED_FACE('',(#465),#375,.T.);
#2069=ADVANCED_FACE('',(#466),#1986,.T.);
#2070=ADVANCED_FACE('',(#467,#319,#320),#376,.T.);
#2071=ADVANCED_FACE('',(#468,#321,#322),#377,.F.);
#2072=ADVANCED_FACE('',(#469),#1987,.F.);
#2073=ADVANCED_FACE('',(#470),#1988,.F.);
#2074=ADVANCED_FACE('',(#471),#378,.T.);
#2075=ADVANCED_FACE('',(#472),#1989,.T.);
#2076=ADVANCED_FACE('',(#473),#379,.T.);
#2077=ADVANCED_FACE('',(#474),#1990,.T.);
#2078=ADVANCED_FACE('',(#475,#323,#324),#380,.T.);
#2079=ADVANCED_FACE('',(#476,#325,#326),#381,.F.);
#2080=ADVANCED_FACE('',(#477),#1991,.T.);
#2081=ADVANCED_FACE('',(#478),#382,.T.);
#2082=ADVANCED_FACE('',(#479),#383,.F.);
#2083=ADVANCED_FACE('',(#480),#1992,.F.);
#2084=ADVANCED_FACE('',(#481),#1993,.T.);
#2085=ADVANCED_FACE('',(#482,#327),#384,.T.);
#2086=ADVANCED_FACE('',(#483,#328),#385,.F.);
#2087=ADVANCED_FACE('',(#484),#1994,.T.);
#2088=ADVANCED_FACE('',(#485,#329),#386,.F.);
#2089=ADVANCED_FACE('',(#486,#330),#387,.F.);
#2090=ADVANCED_FACE('',(#487),#1995,.T.);
#2091=ADVANCED_FACE('',(#488,#331),#388,.T.);
#2092=ADVANCED_FACE('',(#489),#1996,.T.);
#2093=ADVANCED_FACE('',(#490),#389,.F.);
#2094=ADVANCED_FACE('',(#491),#1997,.T.);
#2095=ADVANCED_FACE('',(#492),#390,.T.);
#2096=ADVANCED_FACE('',(#493),#215,.T.);
#2097=ADVANCED_FACE('',(#494),#1998,.T.);
#2098=ADVANCED_FACE('',(#495,#332),#391,.F.);
#2099=ADVANCED_FACE('',(#496),#216,.T.);
#2100=ADVANCED_FACE('',(#497,#333),#392,.T.);
#2101=ADVANCED_FACE('',(#498),#217,.F.);
#2102=ADVANCED_FACE('',(#499),#1999,.F.);
#2103=ADVANCED_FACE('',(#500),#218,.F.);
#2104=ADVANCED_FACE('',(#501),#2000,.F.);
#2105=ADVANCED_FACE('',(#502),#2001,.T.);
#2106=ADVANCED_FACE('',(#503,#334),#393,.T.);
#2107=ADVANCED_FACE('',(#504,#335),#394,.F.);
#2108=ADVANCED_FACE('',(#505),#2002,.T.);
#2109=ADVANCED_FACE('',(#506,#336),#395,.F.);
#2110=ADVANCED_FACE('',(#507,#337),#396,.F.);
#2111=ADVANCED_FACE('',(#508),#2003,.T.);
#2112=ADVANCED_FACE('',(#509,#338),#397,.T.);
#2113=ADVANCED_FACE('',(#510),#2004,.T.);
#2114=ADVANCED_FACE('',(#511),#398,.F.);
#2115=ADVANCED_FACE('',(#512),#2005,.T.);
#2116=ADVANCED_FACE('',(#513),#399,.T.);
#2117=ADVANCED_FACE('',(#514),#2006,.F.);
#2118=ADVANCED_FACE('',(#515),#2007,.T.);
#2119=ADVANCED_FACE('',(#516,#339),#400,.T.);
#2120=ADVANCED_FACE('',(#517,#340),#401,.F.);
#2121=ADVANCED_FACE('',(#518),#402,.F.);
#2122=ADVANCED_FACE('',(#519),#403,.F.);
#2123=ADVANCED_FACE('',(#520),#404,.F.);
#2124=ADVANCED_FACE('',(#521),#2008,.F.);
#2125=ADVANCED_FACE('',(#522),#2009,.T.);
#2126=ADVANCED_FACE('',(#523),#405,.T.);
#2127=ADVANCED_FACE('',(#524),#2010,.T.);
#2128=ADVANCED_FACE('',(#525,#341),#406,.F.);
#2129=ADVANCED_FACE('',(#526,#342),#407,.F.);
#2130=ADVANCED_FACE('',(#527),#2011,.T.);
#2131=ADVANCED_FACE('',(#528,#343),#408,.T.);
#2132=ADVANCED_FACE('',(#529),#2012,.T.);
#2133=ADVANCED_FACE('',(#530),#409,.F.);
#2134=ADVANCED_FACE('',(#531),#2013,.T.);
#2135=ADVANCED_FACE('',(#532),#410,.T.);
#2136=ADVANCED_FACE('',(#533),#2014,.F.);
#2137=ADVANCED_FACE('',(#534),#2015,.T.);
#2138=ADVANCED_FACE('',(#535,#344),#411,.T.);
#2139=ADVANCED_FACE('',(#536,#345),#412,.F.);
#2140=ADVANCED_FACE('',(#537),#2016,.F.);
#2141=ADVANCED_FACE('',(#538),#2017,.T.);
#2142=ADVANCED_FACE('',(#539,#346),#413,.T.);
#2143=ADVANCED_FACE('',(#540,#347),#414,.F.);
#2144=CLOSED_SHELL('',(#2018,#2019,#2020,#2021,#2022,#2023,#2024,#2025,
#2026,#2027));
#2145=CLOSED_SHELL('',(#2028,#2029,#2030,#2031,#2032,#2033,#2034,#2035,
#2036,#2037,#2038));
#2146=CLOSED_SHELL('',(#2039,#2040,#2041,#2042,#2043,#2044,#2045,#2046));
#2147=CLOSED_SHELL('',(#2047,#2048,#2049,#2050,#2051,#2052,#2053,#2054));
#2148=CLOSED_SHELL('',(#2055,#2056,#2057,#2058,#2059,#2060,#2061,#2062,
#2063));
#2149=CLOSED_SHELL('',(#2064,#2065,#2066,#2067,#2068,#2069,#2070,#2071));
#2150=CLOSED_SHELL('',(#2072,#2073,#2074,#2075,#2076,#2077,#2078,#2079));
#2151=CLOSED_SHELL('',(#2080,#2081,#2082));
#2152=CLOSED_SHELL('',(#2083,#2084,#2085,#2086));
#2153=CLOSED_SHELL('',(#2087,#2088,#2089,#2090,#2091,#2092,#2093,#2094,
#2095));
#2154=CLOSED_SHELL('',(#2096,#2097,#2098,#2099,#2100,#2101,#2102,#2103));
#2155=CLOSED_SHELL('',(#2104,#2105,#2106,#2107));
#2156=CLOSED_SHELL('',(#2108,#2109,#2110,#2111,#2112,#2113,#2114,#2115,
#2116));
#2157=CLOSED_SHELL('',(#2117,#2118,#2119,#2120));
#2158=CLOSED_SHELL('',(#2121,#2122,#2123,#2124,#2125,#2126));
#2159=CLOSED_SHELL('',(#2127,#2128,#2129,#2130,#2131,#2132,#2133,#2134,
#2135));
#2160=CLOSED_SHELL('',(#2136,#2137,#2138,#2139));
#2161=CLOSED_SHELL('',(#2140,#2141,#2142,#2143));
#2162=DERIVED_UNIT_ELEMENT(#2198,1.);
#2163=DERIVED_UNIT_ELEMENT(#4050,-3.);
#2164=DERIVED_UNIT_ELEMENT(#2198,1.);
#2165=DERIVED_UNIT_ELEMENT(#4050,-3.);
#2166=DERIVED_UNIT_ELEMENT(#2198,1.);
#2167=DERIVED_UNIT_ELEMENT(#4050,-3.);
#2168=DERIVED_UNIT_ELEMENT(#2198,1.);
#2169=DERIVED_UNIT_ELEMENT(#4050,-3.);
#2170=DERIVED_UNIT_ELEMENT(#2198,1.);
#2171=DERIVED_UNIT_ELEMENT(#4050,-3.);
#2172=DERIVED_UNIT_ELEMENT(#2198,1.);
#2173=DERIVED_UNIT_ELEMENT(#4050,-3.);
#2174=DERIVED_UNIT_ELEMENT(#2198,1.);
#2175=DERIVED_UNIT_ELEMENT(#4050,-3.);
#2176=DERIVED_UNIT_ELEMENT(#2198,1.);
#2177=DERIVED_UNIT_ELEMENT(#4050,-3.);
#2178=DERIVED_UNIT_ELEMENT(#2198,1.);
#2179=DERIVED_UNIT_ELEMENT(#4050,-3.);
#2180=DERIVED_UNIT_ELEMENT(#2198,1.);
#2181=DERIVED_UNIT_ELEMENT(#4050,-3.);
#2182=DERIVED_UNIT_ELEMENT(#2198,1.);
#2183=DERIVED_UNIT_ELEMENT(#4050,-3.);
#2184=DERIVED_UNIT_ELEMENT(#2198,1.);
#2185=DERIVED_UNIT_ELEMENT(#4050,-3.);
#2186=DERIVED_UNIT_ELEMENT(#2198,1.);
#2187=DERIVED_UNIT_ELEMENT(#4050,-3.);
#2188=DERIVED_UNIT_ELEMENT(#2198,1.);
#2189=DERIVED_UNIT_ELEMENT(#4050,-3.);
#2190=DERIVED_UNIT_ELEMENT(#2198,1.);
#2191=DERIVED_UNIT_ELEMENT(#4050,-3.);
#2192=DERIVED_UNIT_ELEMENT(#2198,1.);
#2193=DERIVED_UNIT_ELEMENT(#4050,-3.);
#2194=DERIVED_UNIT_ELEMENT(#2198,1.);
#2195=DERIVED_UNIT_ELEMENT(#4050,-3.);
#2196=DERIVED_UNIT_ELEMENT(#2198,1.);
#2197=DERIVED_UNIT_ELEMENT(#4050,-3.);
#2198=(
MASS_UNIT()
NAMED_UNIT(*)
SI_UNIT(.KILO.,.GRAM.)
);
#2199=DERIVED_UNIT((#2162,#2163));
#2200=DERIVED_UNIT((#2164,#2165));
#2201=DERIVED_UNIT((#2166,#2167));
#2202=DERIVED_UNIT((#2168,#2169));
#2203=DERIVED_UNIT((#2170,#2171));
#2204=DERIVED_UNIT((#2172,#2173));
#2205=DERIVED_UNIT((#2174,#2175));
#2206=DERIVED_UNIT((#2176,#2177));
#2207=DERIVED_UNIT((#2178,#2179));
#2208=DERIVED_UNIT((#2180,#2181));
#2209=DERIVED_UNIT((#2182,#2183));
#2210=DERIVED_UNIT((#2184,#2185));
#2211=DERIVED_UNIT((#2186,#2187));
#2212=DERIVED_UNIT((#2188,#2189));
#2213=DERIVED_UNIT((#2190,#2191));
#2214=DERIVED_UNIT((#2192,#2193));
#2215=DERIVED_UNIT((#2194,#2195));
#2216=DERIVED_UNIT((#2196,#2197));
#2217=MEASURE_REPRESENTATION_ITEM('density measure',
POSITIVE_RATIO_MEASURE(7850.),#2199);
#2218=MEASURE_REPRESENTATION_ITEM('density measure',
POSITIVE_RATIO_MEASURE(7850.),#2200);
#2219=MEASURE_REPRESENTATION_ITEM('density measure',
POSITIVE_RATIO_MEASURE(7850.),#2201);
#2220=MEASURE_REPRESENTATION_ITEM('density measure',
POSITIVE_RATIO_MEASURE(7850.),#2202);
#2221=MEASURE_REPRESENTATION_ITEM('density measure',
POSITIVE_RATIO_MEASURE(7850.),#2203);
#2222=MEASURE_REPRESENTATION_ITEM('density measure',
POSITIVE_RATIO_MEASURE(7850.),#2204);
#2223=MEASURE_REPRESENTATION_ITEM('density measure',
POSITIVE_RATIO_MEASURE(7850.),#2205);
#2224=MEASURE_REPRESENTATION_ITEM('density measure',
POSITIVE_RATIO_MEASURE(1200.),#2206);
#2225=MEASURE_REPRESENTATION_ITEM('density measure',
POSITIVE_RATIO_MEASURE(8920.),#2207);
#2226=MEASURE_REPRESENTATION_ITEM('density measure',
POSITIVE_RATIO_MEASURE(7850.),#2208);
#2227=MEASURE_REPRESENTATION_ITEM('density measure',
POSITIVE_RATIO_MEASURE(7850.),#2209);
#2228=MEASURE_REPRESENTATION_ITEM('density measure',
POSITIVE_RATIO_MEASURE(7850.),#2210);
#2229=MEASURE_REPRESENTATION_ITEM('density measure',
POSITIVE_RATIO_MEASURE(7850.),#2211);
#2230=MEASURE_REPRESENTATION_ITEM('density measure',
POSITIVE_RATIO_MEASURE(7850.),#2212);
#2231=MEASURE_REPRESENTATION_ITEM('density measure',
POSITIVE_RATIO_MEASURE(7850.),#2213);
#2232=MEASURE_REPRESENTATION_ITEM('density measure',
POSITIVE_RATIO_MEASURE(7850.),#2214);
#2233=MEASURE_REPRESENTATION_ITEM('density measure',
POSITIVE_RATIO_MEASURE(8920.),#2215);
#2234=MEASURE_REPRESENTATION_ITEM('density measure',
POSITIVE_RATIO_MEASURE(7850.),#2216);
#2235=PROPERTY_DEFINITION_REPRESENTATION(#2325,#2271);
#2236=PROPERTY_DEFINITION_REPRESENTATION(#2326,#2272);
#2237=PROPERTY_DEFINITION_REPRESENTATION(#2327,#2273);
#2238=PROPERTY_DEFINITION_REPRESENTATION(#2328,#2274);
#2239=PROPERTY_DEFINITION_REPRESENTATION(#2329,#2275);
#2240=PROPERTY_DEFINITION_REPRESENTATION(#2330,#2276);
#2241=PROPERTY_DEFINITION_REPRESENTATION(#2331,#2277);
#2242=PROPERTY_DEFINITION_REPRESENTATION(#2332,#2278);
#2243=PROPERTY_DEFINITION_REPRESENTATION(#2333,#2279);
#2244=PROPERTY_DEFINITION_REPRESENTATION(#2334,#2280);
#2245=PROPERTY_DEFINITION_REPRESENTATION(#2335,#2281);
#2246=PROPERTY_DEFINITION_REPRESENTATION(#2336,#2282);
#2247=PROPERTY_DEFINITION_REPRESENTATION(#2337,#2283);
#2248=PROPERTY_DEFINITION_REPRESENTATION(#2338,#2284);
#2249=PROPERTY_DEFINITION_REPRESENTATION(#2339,#2285);
#2250=PROPERTY_DEFINITION_REPRESENTATION(#2340,#2286);
#2251=PROPERTY_DEFINITION_REPRESENTATION(#2341,#2287);
#2252=PROPERTY_DEFINITION_REPRESENTATION(#2342,#2288);
#2253=PROPERTY_DEFINITION_REPRESENTATION(#2343,#2289);
#2254=PROPERTY_DEFINITION_REPRESENTATION(#2344,#2290);
#2255=PROPERTY_DEFINITION_REPRESENTATION(#2345,#2291);
#2256=PROPERTY_DEFINITION_REPRESENTATION(#2346,#2292);
#2257=PROPERTY_DEFINITION_REPRESENTATION(#2347,#2293);
#2258=PROPERTY_DEFINITION_REPRESENTATION(#2348,#2294);
#2259=PROPERTY_DEFINITION_REPRESENTATION(#2349,#2295);
#2260=PROPERTY_DEFINITION_REPRESENTATION(#2350,#2296);
#2261=PROPERTY_DEFINITION_REPRESENTATION(#2351,#2297);
#2262=PROPERTY_DEFINITION_REPRESENTATION(#2352,#2298);
#2263=PROPERTY_DEFINITION_REPRESENTATION(#2353,#2299);
#2264=PROPERTY_DEFINITION_REPRESENTATION(#2354,#2300);
#2265=PROPERTY_DEFINITION_REPRESENTATION(#2355,#2301);
#2266=PROPERTY_DEFINITION_REPRESENTATION(#2356,#2302);
#2267=PROPERTY_DEFINITION_REPRESENTATION(#2357,#2303);
#2268=PROPERTY_DEFINITION_REPRESENTATION(#2358,#2304);
#2269=PROPERTY_DEFINITION_REPRESENTATION(#2359,#2305);
#2270=PROPERTY_DEFINITION_REPRESENTATION(#2360,#2306);
#2271=REPRESENTATION('material name',(#2307),#4030);
#2272=REPRESENTATION('density',(#2217),#4030);
#2273=REPRESENTATION('material name',(#2308),#4031);
#2274=REPRESENTATION('density',(#2218),#4031);
#2275=REPRESENTATION('material name',(#2309),#4032);
#2276=REPRESENTATION('density',(#2219),#4032);
#2277=REPRESENTATION('material name',(#2310),#4033);
#2278=REPRESENTATION('density',(#2220),#4033);
#2279=REPRESENTATION('material name',(#2311),#4034);
#2280=REPRESENTATION('density',(#2221),#4034);
#2281=REPRESENTATION('material name',(#2312),#4035);
#2282=REPRESENTATION('density',(#2222),#4035);
#2283=REPRESENTATION('material name',(#2313),#4036);
#2284=REPRESENTATION('density',(#2223),#4036);
#2285=REPRESENTATION('material name',(#2314),#4037);
#2286=REPRESENTATION('density',(#2224),#4037);
#2287=REPRESENTATION('material name',(#2315),#4038);
#2288=REPRESENTATION('density',(#2225),#4038);
#2289=REPRESENTATION('material name',(#2316),#4039);
#2290=REPRESENTATION('density',(#2226),#4039);
#2291=REPRESENTATION('material name',(#2317),#4040);
#2292=REPRESENTATION('density',(#2227),#4040);
#2293=REPRESENTATION('material name',(#2318),#4041);
#2294=REPRESENTATION('density',(#2228),#4041);
#2295=REPRESENTATION('material name',(#2319),#4042);
#2296=REPRESENTATION('density',(#2229),#4042);
#2297=REPRESENTATION('material name',(#2320),#4043);
#2298=REPRESENTATION('density',(#2230),#4043);
#2299=REPRESENTATION('material name',(#2321),#4044);
#2300=REPRESENTATION('density',(#2231),#4044);
#2301=REPRESENTATION('material name',(#2322),#4045);
#2302=REPRESENTATION('density',(#2232),#4045);
#2303=REPRESENTATION('material name',(#2323),#4046);
#2304=REPRESENTATION('density',(#2233),#4046);
#2305=REPRESENTATION('material name',(#2324),#4047);
#2306=REPRESENTATION('density',(#2234),#4047);
#2307=DESCRIPTIVE_REPRESENTATION_ITEM('Steel','Steel');
#2308=DESCRIPTIVE_REPRESENTATION_ITEM('Steel','Steel');
#2309=DESCRIPTIVE_REPRESENTATION_ITEM('Steel','Steel');
#2310=DESCRIPTIVE_REPRESENTATION_ITEM('Steel','Steel');
#2311=DESCRIPTIVE_REPRESENTATION_ITEM('Steel','Steel');
#2312=DESCRIPTIVE_REPRESENTATION_ITEM('Steel','Steel');
#2313=DESCRIPTIVE_REPRESENTATION_ITEM('Steel','Steel');
#2314=DESCRIPTIVE_REPRESENTATION_ITEM('Rubber, Nitrile',
'Rubber, Nitrile');
#2315=DESCRIPTIVE_REPRESENTATION_ITEM('Copper, Alloy','Copper, Alloy');
#2316=DESCRIPTIVE_REPRESENTATION_ITEM('Steel','Steel');
#2317=DESCRIPTIVE_REPRESENTATION_ITEM('Steel','Steel');
#2318=DESCRIPTIVE_REPRESENTATION_ITEM('Steel','Steel');
#2319=DESCRIPTIVE_REPRESENTATION_ITEM('Steel','Steel');
#2320=DESCRIPTIVE_REPRESENTATION_ITEM('Steel','Steel');
#2321=DESCRIPTIVE_REPRESENTATION_ITEM('Steel','Steel');
#2322=DESCRIPTIVE_REPRESENTATION_ITEM('Steel','Steel');
#2323=DESCRIPTIVE_REPRESENTATION_ITEM('Copper, Alloy','Copper, Alloy');
#2324=DESCRIPTIVE_REPRESENTATION_ITEM('Steel','Steel');
#2325=PROPERTY_DEFINITION('material property','material name',#4163);
#2326=PROPERTY_DEFINITION('material property','density of part',#4163);
#2327=PROPERTY_DEFINITION('material property','material name',#4164);
#2328=PROPERTY_DEFINITION('material property','density of part',#4164);
#2329=PROPERTY_DEFINITION('material property','material name',#4165);
#2330=PROPERTY_DEFINITION('material property','density of part',#4165);
#2331=PROPERTY_DEFINITION('material property','material name',#4166);
#2332=PROPERTY_DEFINITION('material property','density of part',#4166);
#2333=PROPERTY_DEFINITION('material property','material name',#4167);
#2334=PROPERTY_DEFINITION('material property','density of part',#4167);
#2335=PROPERTY_DEFINITION('material property','material name',#4168);
#2336=PROPERTY_DEFINITION('material property','density of part',#4168);
#2337=PROPERTY_DEFINITION('material property','material name',#4169);
#2338=PROPERTY_DEFINITION('material property','density of part',#4169);
#2339=PROPERTY_DEFINITION('material property','material name',#4170);
#2340=PROPERTY_DEFINITION('material property','density of part',#4170);
#2341=PROPERTY_DEFINITION('material property','material name',#4171);
#2342=PROPERTY_DEFINITION('material property','density of part',#4171);
#2343=PROPERTY_DEFINITION('material property','material name',#4172);
#2344=PROPERTY_DEFINITION('material property','density of part',#4172);
#2345=PROPERTY_DEFINITION('material property','material name',#4173);
#2346=PROPERTY_DEFINITION('material property','density of part',#4173);
#2347=PROPERTY_DEFINITION('material property','material name',#4174);
#2348=PROPERTY_DEFINITION('material property','density of part',#4174);
#2349=PROPERTY_DEFINITION('material property','material name',#4175);
#2350=PROPERTY_DEFINITION('material property','density of part',#4175);
#2351=PROPERTY_DEFINITION('material property','material name',#4176);
#2352=PROPERTY_DEFINITION('material property','density of part',#4176);
#2353=PROPERTY_DEFINITION('material property','material name',#4177);
#2354=PROPERTY_DEFINITION('material property','density of part',#4177);
#2355=PROPERTY_DEFINITION('material property','material name',#4178);
#2356=PROPERTY_DEFINITION('material property','density of part',#4178);
#2357=PROPERTY_DEFINITION('material property','material name',#4179);
#2358=PROPERTY_DEFINITION('material property','density of part',#4179);
#2359=PROPERTY_DEFINITION('material property','material name',#4180);
#2360=PROPERTY_DEFINITION('material property','density of part',#4180);
#2361=AXIS2_PLACEMENT_3D('',#3416,#2671,#2672);
#2362=AXIS2_PLACEMENT_3D('',#3417,#2673,#2674);
#2363=AXIS2_PLACEMENT_3D('',#3418,#2675,#2676);
#2364=AXIS2_PLACEMENT_3D('',#3420,#2677,#2678);
#2365=AXIS2_PLACEMENT_3D('',#3423,#2680,#2681);
#2366=AXIS2_PLACEMENT_3D('',#3424,#2682,#2683);
#2367=AXIS2_PLACEMENT_3D('',#3426,#2684,#2685);
#2368=AXIS2_PLACEMENT_3D('',#3429,#2687,#2688);
#2369=AXIS2_PLACEMENT_3D('',#3430,#2689,#2690);
#2370=AXIS2_PLACEMENT_3D('',#3432,#2691,#2692);
#2371=AXIS2_PLACEMENT_3D('',#3435,#2694,#2695);
#2372=AXIS2_PLACEMENT_3D('',#3436,#2696,#2697);
#2373=AXIS2_PLACEMENT_3D('',#3438,#2698,#2699);
#2374=AXIS2_PLACEMENT_3D('',#3441,#2701,#2702);
#2375=AXIS2_PLACEMENT_3D('',#3442,#2703,#2704);
#2376=AXIS2_PLACEMENT_3D('',#3451,#2709,#2710);
#2377=AXIS2_PLACEMENT_3D('',#3457,#2714,#2715);
#2378=AXIS2_PLACEMENT_3D('',#3463,#2719,#2720);
#2379=AXIS2_PLACEMENT_3D('',#3466,#2723,#2724);
#2380=AXIS2_PLACEMENT_3D('',#3467,#2725,#2726);
#2381=AXIS2_PLACEMENT_3D('',#3468,#2727,#2728);
#2382=AXIS2_PLACEMENT_3D('',#3469,#2729,#2730);
#2383=AXIS2_PLACEMENT_3D('',#3471,#2731,#2732);
#2384=AXIS2_PLACEMENT_3D('',#3474,#2734,#2735);
#2385=AXIS2_PLACEMENT_3D('',#3475,#2736,#2737);
#2386=AXIS2_PLACEMENT_3D('',#3477,#2738,#2739);
#2387=AXIS2_PLACEMENT_3D('',#3480,#2741,#2742);
#2388=AXIS2_PLACEMENT_3D('',#3481,#2743,#2744);
#2389=AXIS2_PLACEMENT_3D('',#3483,#2745,#2746);
#2390=AXIS2_PLACEMENT_3D('',#3486,#2748,#2749);
#2391=AXIS2_PLACEMENT_3D('',#3487,#2750,#2751);
#2392=AXIS2_PLACEMENT_3D('',#3496,#2756,#2757);
#2393=AXIS2_PLACEMENT_3D('',#3502,#2761,#2762);
#2394=AXIS2_PLACEMENT_3D('',#3508,#2766,#2767);
#2395=AXIS2_PLACEMENT_3D('',#3517,#2772,#2773);
#2396=AXIS2_PLACEMENT_3D('',#3520,#2776,#2777);
#2397=AXIS2_PLACEMENT_3D('',#3523,#2780,#2781);
#2398=AXIS2_PLACEMENT_3D('',#3524,#2782,#2783);
#2399=AXIS2_PLACEMENT_3D('',#3525,#2784,#2785);
#2400=AXIS2_PLACEMENT_3D('',#3526,#2786,#2787);
#2401=AXIS2_PLACEMENT_3D('',#3528,#2788,#2789);
#2402=AXIS2_PLACEMENT_3D('',#3531,#2791,#2792);
#2403=AXIS2_PLACEMENT_3D('',#3532,#2793,#2794);
#2404=AXIS2_PLACEMENT_3D('',#3534,#2795,#2796);
#2405=AXIS2_PLACEMENT_3D('',#3537,#2798,#2799);
#2406=AXIS2_PLACEMENT_3D('',#3538,#2800,#2801);
#2407=AXIS2_PLACEMENT_3D('',#3547,#2806,#2807);
#2408=AXIS2_PLACEMENT_3D('',#3549,#2808,#2809);
#2409=AXIS2_PLACEMENT_3D('',#3551,#2810,#2811);
#2410=AXIS2_PLACEMENT_3D('',#3553,#2813,#2814);
#2411=AXIS2_PLACEMENT_3D('',#3559,#2818,#2819);
#2412=AXIS2_PLACEMENT_3D('',#3560,#2820,#2821);
#2413=AXIS2_PLACEMENT_3D('',#3561,#2822,#2823);
#2414=AXIS2_PLACEMENT_3D('',#3562,#2824,#2825);
#2415=AXIS2_PLACEMENT_3D('',#3563,#2826,#2827);
#2416=AXIS2_PLACEMENT_3D('',#3564,#2828,#2829);
#2417=AXIS2_PLACEMENT_3D('',#3565,#2830,#2831);
#2418=AXIS2_PLACEMENT_3D('',#3567,#2832,#2833);
#2419=AXIS2_PLACEMENT_3D('',#3570,#2835,#2836);
#2420=AXIS2_PLACEMENT_3D('',#3571,#2837,#2838);
#2421=AXIS2_PLACEMENT_3D('',#3573,#2839,#2840);
#2422=AXIS2_PLACEMENT_3D('',#3576,#2842,#2843);
#2423=AXIS2_PLACEMENT_3D('',#3577,#2844,#2845);
#2424=AXIS2_PLACEMENT_3D('',#3586,#2850,#2851);
#2425=AXIS2_PLACEMENT_3D('',#3588,#2852,#2853);
#2426=AXIS2_PLACEMENT_3D('',#3590,#2854,#2855);
#2427=AXIS2_PLACEMENT_3D('',#3592,#2857,#2858);
#2428=AXIS2_PLACEMENT_3D('',#3598,#2862,#2863);
#2429=AXIS2_PLACEMENT_3D('',#3599,#2864,#2865);
#2430=AXIS2_PLACEMENT_3D('',#3600,#2866,#2867);
#2431=AXIS2_PLACEMENT_3D('',#3601,#2868,#2869);
#2432=AXIS2_PLACEMENT_3D('',#3602,#2870,#2871);
#2433=AXIS2_PLACEMENT_3D('',#3603,#2872,#2873);
#2434=AXIS2_PLACEMENT_3D('',#3604,#2874,#2875);
#2435=AXIS2_PLACEMENT_3D('',#3606,#2876,#2877);
#2436=AXIS2_PLACEMENT_3D('',#3609,#2879,#2880);
#2437=AXIS2_PLACEMENT_3D('',#3610,#2881,#2882);
#2438=AXIS2_PLACEMENT_3D('',#3612,#2883,#2884);
#2439=AXIS2_PLACEMENT_3D('',#3615,#2886,#2887);
#2440=AXIS2_PLACEMENT_3D('',#3616,#2888,#2889);
#2441=AXIS2_PLACEMENT_3D('',#3618,#2890,#2891);
#2442=AXIS2_PLACEMENT_3D('',#3621,#2893,#2894);
#2443=AXIS2_PLACEMENT_3D('',#3622,#2895,#2896);
#2444=AXIS2_PLACEMENT_3D('',#3631,#2901,#2902);
#2445=AXIS2_PLACEMENT_3D('',#3633,#2903,#2904);
#2446=AXIS2_PLACEMENT_3D('',#3635,#2905,#2906);
#2447=AXIS2_PLACEMENT_3D('',#3637,#2908,#2909);
#2448=AXIS2_PLACEMENT_3D('',#3643,#2913,#2914);
#2449=AXIS2_PLACEMENT_3D('',#3644,#2915,#2916);
#2450=AXIS2_PLACEMENT_3D('',#3645,#2917,#2918);
#2451=AXIS2_PLACEMENT_3D('',#3646,#2919,#2920);
#2452=AXIS2_PLACEMENT_3D('',#3647,#2921,#2922);
#2453=AXIS2_PLACEMENT_3D('',#3648,#2923,#2924);
#2454=AXIS2_PLACEMENT_3D('',#3649,#2925,#2926);
#2455=AXIS2_PLACEMENT_3D('',#3651,#2927,#2928);
#2456=AXIS2_PLACEMENT_3D('',#3654,#2930,#2931);
#2457=AXIS2_PLACEMENT_3D('',#3655,#2932,#2933);
#2458=AXIS2_PLACEMENT_3D('',#3657,#2934,#2935);
#2459=AXIS2_PLACEMENT_3D('',#3660,#2937,#2938);
#2460=AXIS2_PLACEMENT_3D('',#3661,#2939,#2940);
#2461=AXIS2_PLACEMENT_3D('',#3670,#2945,#2946);
#2462=AXIS2_PLACEMENT_3D('',#3672,#2947,#2948);
#2463=AXIS2_PLACEMENT_3D('',#3674,#2949,#2950);
#2464=AXIS2_PLACEMENT_3D('',#3676,#2952,#2953);
#2465=AXIS2_PLACEMENT_3D('',#3682,#2957,#2958);
#2466=AXIS2_PLACEMENT_3D('',#3683,#2959,#2960);
#2467=AXIS2_PLACEMENT_3D('',#3684,#2961,#2962);
#2468=AXIS2_PLACEMENT_3D('',#3685,#2963,#2964);
#2469=AXIS2_PLACEMENT_3D('',#3686,#2965,#2966);
#2470=AXIS2_PLACEMENT_3D('',#3687,#2967,#2968);
#2471=AXIS2_PLACEMENT_3D('',#3688,#2969,#2970);
#2472=AXIS2_PLACEMENT_3D('',#3690,#2971,#2972);
#2473=AXIS2_PLACEMENT_3D('',#3693,#2974,#2975);
#2474=AXIS2_PLACEMENT_3D('',#3694,#2976,#2977);
#2475=AXIS2_PLACEMENT_3D('',#3696,#2978,#2979);
#2476=AXIS2_PLACEMENT_3D('',#3699,#2981,#2982);
#2477=AXIS2_PLACEMENT_3D('',#3700,#2983,#2984);
#2478=AXIS2_PLACEMENT_3D('',#3709,#2989,#2990);
#2479=AXIS2_PLACEMENT_3D('',#3711,#2991,#2992);
#2480=AXIS2_PLACEMENT_3D('',#3713,#2993,#2994);
#2481=AXIS2_PLACEMENT_3D('',#3715,#2996,#2997);
#2482=AXIS2_PLACEMENT_3D('',#3721,#3001,#3002);
#2483=AXIS2_PLACEMENT_3D('',#3722,#3003,#3004);
#2484=AXIS2_PLACEMENT_3D('',#3723,#3005,#3006);
#2485=AXIS2_PLACEMENT_3D('',#3724,#3007,#3008);
#2486=AXIS2_PLACEMENT_3D('',#3725,#3009,#3010);
#2487=AXIS2_PLACEMENT_3D('',#3726,#3011,#3012);
#2488=AXIS2_PLACEMENT_3D('',#3727,#3013,#3014);
#2489=AXIS2_PLACEMENT_3D('',#3729,#3015,#3016);
#2490=AXIS2_PLACEMENT_3D('',#3732,#3018,#3019);
#2491=AXIS2_PLACEMENT_3D('',#3733,#3020,#3021);
#2492=AXIS2_PLACEMENT_3D('',#3734,#3022,#3023);
#2493=AXIS2_PLACEMENT_3D('',#3735,#3024,#3025);
#2494=AXIS2_PLACEMENT_3D('',#3736,#3026,#3027);
#2495=AXIS2_PLACEMENT_3D('',#3738,#3028,#3029);
#2496=AXIS2_PLACEMENT_3D('',#3741,#3031,#3032);
#2497=AXIS2_PLACEMENT_3D('',#3742,#3033,#3034);
#2498=AXIS2_PLACEMENT_3D('',#3744,#3035,#3036);
#2499=AXIS2_PLACEMENT_3D('',#3747,#3038,#3039);
#2500=AXIS2_PLACEMENT_3D('',#3748,#3040,#3041);
#2501=AXIS2_PLACEMENT_3D('',#3749,#3042,#3043);
#2502=AXIS2_PLACEMENT_3D('',#3750,#3044,#3045);
#2503=AXIS2_PLACEMENT_3D('',#3751,#3046,#3047);
#2504=AXIS2_PLACEMENT_3D('',#3753,#3048,#3049);
#2505=AXIS2_PLACEMENT_3D('',#3756,#3051,#3052);
#2506=AXIS2_PLACEMENT_3D('',#3757,#3053,#3054);
#2507=AXIS2_PLACEMENT_3D('',#3759,#3055,#3056);
#2508=AXIS2_PLACEMENT_3D('',#3760,#3057,#3058);
#2509=AXIS2_PLACEMENT_3D('',#3762,#3059,#3060);
#2510=AXIS2_PLACEMENT_3D('',#3763,#3061,#3062);
#2511=AXIS2_PLACEMENT_3D('',#3765,#3063,#3064);
#2512=AXIS2_PLACEMENT_3D('',#3767,#3066,#3067);
#2513=AXIS2_PLACEMENT_3D('',#3769,#3068,#3069);
#2514=AXIS2_PLACEMENT_3D('',#3771,#3070,#3071);
#2515=AXIS2_PLACEMENT_3D('',#3772,#3072,#3073);
#2516=AXIS2_PLACEMENT_3D('',#3775,#3075,#3076);
#2517=AXIS2_PLACEMENT_3D('',#3776,#3077,#3078);
#2518=AXIS2_PLACEMENT_3D('',#3777,#3079,#3080);
#2519=AXIS2_PLACEMENT_3D('',#3779,#3082,#3083);
#2520=AXIS2_PLACEMENT_3D('',#3780,#3084,#3085);
#2521=AXIS2_PLACEMENT_3D('',#3781,#3086,#3087);
#2522=AXIS2_PLACEMENT_3D('',#3783,#3088,#3089);
#2523=AXIS2_PLACEMENT_3D('',#3786,#3091,#3092);
#2524=AXIS2_PLACEMENT_3D('',#3787,#3093,#3094);
#2525=AXIS2_PLACEMENT_3D('',#3789,#3095,#3096);
#2526=AXIS2_PLACEMENT_3D('',#3791,#3098,#3099);
#2527=AXIS2_PLACEMENT_3D('',#3793,#3100,#3101);
#2528=AXIS2_PLACEMENT_3D('',#3794,#3102,#3103);
#2529=AXIS2_PLACEMENT_3D('',#3796,#3104,#3105);
#2530=AXIS2_PLACEMENT_3D('',#3798,#3107,#3108);
#2531=AXIS2_PLACEMENT_3D('',#3800,#3109,#3110);
#2532=AXIS2_PLACEMENT_3D('',#3801,#3111,#3112);
#2533=AXIS2_PLACEMENT_3D('',#3803,#3113,#3114);
#2534=AXIS2_PLACEMENT_3D('',#3805,#3116,#3117);
#2535=AXIS2_PLACEMENT_3D('',#3807,#3118,#3119);
#2536=AXIS2_PLACEMENT_3D('',#3809,#3121,#3122);
#2537=AXIS2_PLACEMENT_3D('',#3811,#3124,#3125);
#2538=AXIS2_PLACEMENT_3D('',#3812,#3126,#3127);
#2539=AXIS2_PLACEMENT_3D('',#3814,#3128,#3129);
#2540=AXIS2_PLACEMENT_3D('',#3817,#3131,#3132);
#2541=AXIS2_PLACEMENT_3D('',#3818,#3133,#3134);
#2542=AXIS2_PLACEMENT_3D('',#3820,#3135,#3136);
#2543=AXIS2_PLACEMENT_3D('',#3823,#3138,#3139);
#2544=AXIS2_PLACEMENT_3D('',#3824,#3140,#3141);
#2545=AXIS2_PLACEMENT_3D('',#3825,#3142,#3143);
#2546=AXIS2_PLACEMENT_3D('',#3826,#3144,#3145);
#2547=AXIS2_PLACEMENT_3D('',#3827,#3146,#3147);
#2548=AXIS2_PLACEMENT_3D('',#3829,#3148,#3149);
#2549=AXIS2_PLACEMENT_3D('',#3832,#3151,#3152);
#2550=AXIS2_PLACEMENT_3D('',#3833,#3153,#3154);
#2551=AXIS2_PLACEMENT_3D('',#3835,#3155,#3156);
#2552=AXIS2_PLACEMENT_3D('',#3836,#3157,#3158);
#2553=AXIS2_PLACEMENT_3D('',#3838,#3159,#3160);
#2554=AXIS2_PLACEMENT_3D('',#3839,#3161,#3162);
#2555=AXIS2_PLACEMENT_3D('',#3841,#3163,#3164);
#2556=AXIS2_PLACEMENT_3D('',#3843,#3166,#3167);
#2557=AXIS2_PLACEMENT_3D('',#3845,#3168,#3169);
#2558=AXIS2_PLACEMENT_3D('',#3847,#3170,#3171);
#2559=AXIS2_PLACEMENT_3D('',#3848,#3172,#3173);
#2560=AXIS2_PLACEMENT_3D('',#3851,#3175,#3176);
#2561=AXIS2_PLACEMENT_3D('',#3852,#3177,#3178);
#2562=AXIS2_PLACEMENT_3D('',#3853,#3179,#3180);
#2563=AXIS2_PLACEMENT_3D('',#3855,#3182,#3183);
#2564=AXIS2_PLACEMENT_3D('',#3856,#3184,#3185);
#2565=AXIS2_PLACEMENT_3D('',#3857,#3186,#3187);
#2566=AXIS2_PLACEMENT_3D('',#3859,#3188,#3189);
#2567=AXIS2_PLACEMENT_3D('',#3862,#3191,#3192);
#2568=AXIS2_PLACEMENT_3D('',#3863,#3193,#3194);
#2569=AXIS2_PLACEMENT_3D('',#3865,#3195,#3196);
#2570=AXIS2_PLACEMENT_3D('',#3868,#3198,#3199);
#2571=AXIS2_PLACEMENT_3D('',#3869,#3200,#3201);
#2572=AXIS2_PLACEMENT_3D('',#3870,#3202,#3203);
#2573=AXIS2_PLACEMENT_3D('',#3871,#3204,#3205);
#2574=AXIS2_PLACEMENT_3D('',#3872,#3206,#3207);
#2575=AXIS2_PLACEMENT_3D('',#3881,#3212,#3213);
#2576=AXIS2_PLACEMENT_3D('',#3890,#3218,#3219);
#2577=AXIS2_PLACEMENT_3D('',#3891,#3220,#3221);
#2578=AXIS2_PLACEMENT_3D('',#3892,#3222,#3223);
#2579=AXIS2_PLACEMENT_3D('',#3893,#3224,#3225);
#2580=AXIS2_PLACEMENT_3D('',#3894,#3226,#3227);
#2581=AXIS2_PLACEMENT_3D('',#3895,#3228,#3229);
#2582=AXIS2_PLACEMENT_3D('',#3896,#3230,#3231);
#2583=AXIS2_PLACEMENT_3D('',#3897,#3232,#3233);
#2584=AXIS2_PLACEMENT_3D('',#3898,#3234,#3235);
#2585=AXIS2_PLACEMENT_3D('',#3899,#3236,#3237);
#2586=AXIS2_PLACEMENT_3D('',#3901,#3238,#3239);
#2587=AXIS2_PLACEMENT_3D('',#3904,#3241,#3242);
#2588=AXIS2_PLACEMENT_3D('',#3905,#3243,#3244);
#2589=AXIS2_PLACEMENT_3D('',#3907,#3245,#3246);
#2590=AXIS2_PLACEMENT_3D('',#3908,#3247,#3248);
#2591=AXIS2_PLACEMENT_3D('',#3910,#3249,#3250);
#2592=AXIS2_PLACEMENT_3D('',#3911,#3251,#3252);
#2593=AXIS2_PLACEMENT_3D('',#3913,#3253,#3254);
#2594=AXIS2_PLACEMENT_3D('',#3915,#3256,#3257);
#2595=AXIS2_PLACEMENT_3D('',#3917,#3258,#3259);
#2596=AXIS2_PLACEMENT_3D('',#3919,#3260,#3261);
#2597=AXIS2_PLACEMENT_3D('',#3920,#3262,#3263);
#2598=AXIS2_PLACEMENT_3D('',#3923,#3265,#3266);
#2599=AXIS2_PLACEMENT_3D('',#3924,#3267,#3268);
#2600=AXIS2_PLACEMENT_3D('',#3925,#3269,#3270);
#2601=AXIS2_PLACEMENT_3D('',#3927,#3272,#3273);
#2602=AXIS2_PLACEMENT_3D('',#3928,#3274,#3275);
#2603=AXIS2_PLACEMENT_3D('',#3929,#3276,#3277);
#2604=AXIS2_PLACEMENT_3D('',#3931,#3278,#3279);
#2605=AXIS2_PLACEMENT_3D('',#3934,#3281,#3282);
#2606=AXIS2_PLACEMENT_3D('',#3935,#3283,#3284);
#2607=AXIS2_PLACEMENT_3D('',#3937,#3285,#3286);
#2608=AXIS2_PLACEMENT_3D('',#3940,#3288,#3289);
#2609=AXIS2_PLACEMENT_3D('',#3941,#3290,#3291);
#2610=AXIS2_PLACEMENT_3D('',#3942,#3292,#3293);
#2611=AXIS2_PLACEMENT_3D('',#3943,#3294,#3295);
#2612=AXIS2_PLACEMENT_3D('',#3944,#3296,#3297);
#2613=AXIS2_PLACEMENT_3D('',#3946,#3298,#3299);
#2614=AXIS2_PLACEMENT_3D('',#3949,#3301,#3302);
#2615=AXIS2_PLACEMENT_3D('',#3950,#3303,#3304);
#2616=AXIS2_PLACEMENT_3D('',#3952,#3305,#3306);
#2617=AXIS2_PLACEMENT_3D('',#3955,#3308,#3309);
#2618=AXIS2_PLACEMENT_3D('',#3956,#3310,#3311);
#2619=AXIS2_PLACEMENT_3D('',#3957,#3312,#3313);
#2620=AXIS2_PLACEMENT_3D('',#3958,#3314,#3315);
#2621=AXIS2_PLACEMENT_3D('',#3959,#3316,#3317);
#2622=AXIS2_PLACEMENT_3D('',#3960,#3318,#3319);
#2623=AXIS2_PLACEMENT_3D('',#3961,#3320,#3321);
#2624=AXIS2_PLACEMENT_3D('',#3962,#3322,#3323);
#2625=AXIS2_PLACEMENT_3D('',#3963,#3324,#3325);
#2626=AXIS2_PLACEMENT_3D('',#3964,#3326,#3327);
#2627=AXIS2_PLACEMENT_3D('',#3965,#3328,#3329);
#2628=AXIS2_PLACEMENT_3D('',#3966,#3330,#3331);
#2629=AXIS2_PLACEMENT_3D('',#3967,#3332,#3333);
#2630=AXIS2_PLACEMENT_3D('',#3968,#3334,#3335);
#2631=AXIS2_PLACEMENT_3D('',#3969,#3336,#3337);
#2632=AXIS2_PLACEMENT_3D('',#3970,#3338,#3339);
#2633=AXIS2_PLACEMENT_3D('',#3971,#3340,#3341);
#2634=AXIS2_PLACEMENT_3D('',#3972,#3342,#3343);
#2635=AXIS2_PLACEMENT_3D('',#3973,#3344,#3345);
#2636=AXIS2_PLACEMENT_3D('',#3974,#3346,#3347);
#2637=AXIS2_PLACEMENT_3D('',#3975,#3348,#3349);
#2638=AXIS2_PLACEMENT_3D('',#3976,#3350,#3351);
#2639=AXIS2_PLACEMENT_3D('',#3977,#3352,#3353);
#2640=AXIS2_PLACEMENT_3D('',#3978,#3354,#3355);
#2641=AXIS2_PLACEMENT_3D('',#3979,#3356,#3357);
#2642=AXIS2_PLACEMENT_3D('',#3980,#3358,#3359);
#2643=AXIS2_PLACEMENT_3D('',#3981,#3360,#3361);
#2644=AXIS2_PLACEMENT_3D('',#3982,#3362,#3363);
#2645=AXIS2_PLACEMENT_3D('',#3983,#3364,#3365);
#2646=AXIS2_PLACEMENT_3D('',#3984,#3366,#3367);
#2647=AXIS2_PLACEMENT_3D('',#3985,#3368,#3369);
#2648=AXIS2_PLACEMENT_3D('',#3986,#3370,#3371);
#2649=AXIS2_PLACEMENT_3D('',#3987,#3372,#3373);
#2650=AXIS2_PLACEMENT_3D('',#3988,#3374,#3375);
#2651=AXIS2_PLACEMENT_3D('',#3989,#3376,#3377);
#2652=AXIS2_PLACEMENT_3D('',#3990,#3378,#3379);
#2653=AXIS2_PLACEMENT_3D('',#3991,#3380,#3381);
#2654=AXIS2_PLACEMENT_3D('',#3992,#3382,#3383);
#2655=AXIS2_PLACEMENT_3D('',#3993,#3384,#3385);
#2656=AXIS2_PLACEMENT_3D('',#3994,#3386,#3387);
#2657=AXIS2_PLACEMENT_3D('',#3995,#3388,#3389);
#2658=AXIS2_PLACEMENT_3D('',#3996,#3390,#3391);
#2659=AXIS2_PLACEMENT_3D('',#3997,#3392,#3393);
#2660=AXIS2_PLACEMENT_3D('',#3998,#3394,#3395);
#2661=AXIS2_PLACEMENT_3D('',#3999,#3396,#3397);
#2662=AXIS2_PLACEMENT_3D('',#4000,#3398,#3399);
#2663=AXIS2_PLACEMENT_3D('',#4001,#3400,#3401);
#2664=AXIS2_PLACEMENT_3D('',#4002,#3402,#3403);
#2665=AXIS2_PLACEMENT_3D('',#4003,#3404,#3405);
#2666=AXIS2_PLACEMENT_3D('',#4004,#3406,#3407);
#2667=AXIS2_PLACEMENT_3D('',#4005,#3408,#3409);
#2668=AXIS2_PLACEMENT_3D('',#4006,#3410,#3411);
#2669=AXIS2_PLACEMENT_3D('',#4007,#3412,#3413);
#2670=AXIS2_PLACEMENT_3D('',#4008,#3414,#3415);
#2671=DIRECTION('axis',(0.,0.,1.));
#2672=DIRECTION('refdir',(1.,0.,0.));
#2673=DIRECTION('axis',(0.,0.,1.));
#2674=DIRECTION('refdir',(1.,0.,0.));
#2675=DIRECTION('center_axis',(0.,0.,-1.));
#2676=DIRECTION('ref_axis',(1.,0.,0.));
#2677=DIRECTION('center_axis',(0.,0.,-1.));
#2678=DIRECTION('ref_axis',(1.,0.,0.));
#2679=DIRECTION('',(0.,0.,-1.));
#2680=DIRECTION('center_axis',(0.,0.,1.));
#2681=DIRECTION('ref_axis',(1.,0.,0.));
#2682=DIRECTION('center_axis',(0.,0.,-1.));
#2683=DIRECTION('ref_axis',(1.,0.,0.));
#2684=DIRECTION('center_axis',(0.,0.,-1.));
#2685=DIRECTION('ref_axis',(1.,0.,0.));
#2686=DIRECTION('',(0.,0.,-1.));
#2687=DIRECTION('center_axis',(0.,0.,1.));
#2688=DIRECTION('ref_axis',(1.,0.,0.));
#2689=DIRECTION('center_axis',(0.,0.,-1.));
#2690=DIRECTION('ref_axis',(1.,0.,0.));
#2691=DIRECTION('center_axis',(0.,0.,-1.));
#2692=DIRECTION('ref_axis',(1.,0.,0.));
#2693=DIRECTION('',(0.,0.,-1.));
#2694=DIRECTION('center_axis',(0.,0.,1.));
#2695=DIRECTION('ref_axis',(1.,0.,0.));
#2696=DIRECTION('center_axis',(0.,0.,-1.));
#2697=DIRECTION('ref_axis',(1.,0.,0.));
#2698=DIRECTION('center_axis',(0.,0.,-1.));
#2699=DIRECTION('ref_axis',(1.,0.,0.));
#2700=DIRECTION('',(0.,0.,-1.));
#2701=DIRECTION('center_axis',(0.,0.,1.));
#2702=DIRECTION('ref_axis',(1.,0.,0.));
#2703=DIRECTION('center_axis',(0.,1.,0.));
#2704=DIRECTION('ref_axis',(-1.,0.,0.));
#2705=DIRECTION('',(1.,0.,0.));
#2706=DIRECTION('',(0.,0.,1.));
#2707=DIRECTION('',(1.,0.,0.));
#2708=DIRECTION('',(0.,0.,1.));
#2709=DIRECTION('center_axis',(1.,0.,0.));
#2710=DIRECTION('ref_axis',(0.,1.,0.));
#2711=DIRECTION('',(0.,-1.,0.));
#2712=DIRECTION('',(0.,-1.,0.));
#2713=DIRECTION('',(0.,0.,1.));
#2714=DIRECTION('center_axis',(0.,-1.,0.));
#2715=DIRECTION('ref_axis',(1.,0.,0.));
#2716=DIRECTION('',(-1.,0.,0.));
#2717=DIRECTION('',(-1.,0.,0.));
#2718=DIRECTION('',(0.,0.,-1.));
#2719=DIRECTION('center_axis',(-1.,0.,0.));
#2720=DIRECTION('ref_axis',(0.,-1.,0.));
#2721=DIRECTION('',(0.,1.,0.));
#2722=DIRECTION('',(0.,1.,0.));
#2723=DIRECTION('center_axis',(0.,0.,1.));
#2724=DIRECTION('ref_axis',(1.,0.,0.));
#2725=DIRECTION('center_axis',(0.,0.,1.));
#2726=DIRECTION('ref_axis',(1.,0.,0.));
#2727=DIRECTION('axis',(0.,0.,1.));
#2728=DIRECTION('refdir',(1.,0.,0.));
#2729=DIRECTION('center_axis',(0.,0.,-1.));
#2730=DIRECTION('ref_axis',(1.,0.,0.));
#2731=DIRECTION('center_axis',(0.,0.,-1.));
#2732=DIRECTION('ref_axis',(1.,0.,0.));
#2733=DIRECTION('',(0.,0.,-1.));
#2734=DIRECTION('center_axis',(0.,0.,1.));
#2735=DIRECTION('ref_axis',(1.,0.,0.));
#2736=DIRECTION('center_axis',(0.,0.,-1.));
#2737=DIRECTION('ref_axis',(1.,0.,0.));
#2738=DIRECTION('center_axis',(0.,0.,-1.));
#2739=DIRECTION('ref_axis',(1.,0.,0.));
#2740=DIRECTION('',(0.,0.,-1.));
#2741=DIRECTION('center_axis',(0.,0.,1.));
#2742=DIRECTION('ref_axis',(1.,0.,0.));
#2743=DIRECTION('center_axis',(0.,0.,-1.));
#2744=DIRECTION('ref_axis',(1.,0.,0.));
#2745=DIRECTION('center_axis',(0.,0.,-1.));
#2746=DIRECTION('ref_axis',(1.,0.,0.));
#2747=DIRECTION('',(0.,0.,-1.));
#2748=DIRECTION('center_axis',(0.,0.,1.));
#2749=DIRECTION('ref_axis',(1.,0.,0.));
#2750=DIRECTION('center_axis',(1.,0.,0.));
#2751=DIRECTION('ref_axis',(0.,1.,0.));
#2752=DIRECTION('',(0.,1.,0.));
#2753=DIRECTION('',(0.,0.,-1.));
#2754=DIRECTION('',(0.,1.,0.));
#2755=DIRECTION('',(0.,0.,1.));
#2756=DIRECTION('center_axis',(0.,-1.,0.));
#2757=DIRECTION('ref_axis',(1.,0.,0.));
#2758=DIRECTION('',(1.,0.,0.));
#2759=DIRECTION('',(1.,0.,0.));
#2760=DIRECTION('',(0.,0.,1.));
#2761=DIRECTION('center_axis',(0.,-1.,0.));
#2762=DIRECTION('ref_axis',(1.,0.,0.));
#2763=DIRECTION('',(1.,0.,0.));
#2764=DIRECTION('',(0.,0.,-1.));
#2765=DIRECTION('',(1.,0.,0.));
#2766=DIRECTION('center_axis',(0.,1.,0.));
#2767=DIRECTION('ref_axis',(-1.,0.,0.));
#2768=DIRECTION('',(1.,0.,0.));
#2769=DIRECTION('',(0.,0.,-1.));
#2770=DIRECTION('',(1.,0.,0.));
#2771=DIRECTION('',(0.,0.,-1.));
#2772=DIRECTION('center_axis',(1.,0.,0.));
#2773=DIRECTION('ref_axis',(0.,1.,0.));
#2774=DIRECTION('',(0.,-1.,0.));
#2775=DIRECTION('',(0.,-1.,0.));
#2776=DIRECTION('center_axis',(-1.,0.,0.));
#2777=DIRECTION('ref_axis',(0.,-1.,0.));
#2778=DIRECTION('',(0.,1.,0.));
#2779=DIRECTION('',(0.,1.,0.));
#2780=DIRECTION('center_axis',(0.,0.,1.));
#2781=DIRECTION('ref_axis',(1.,0.,0.));
#2782=DIRECTION('center_axis',(0.,0.,1.));
#2783=DIRECTION('ref_axis',(1.,0.,0.));
#2784=DIRECTION('axis',(0.,0.,1.));
#2785=DIRECTION('refdir',(1.,0.,0.));
#2786=DIRECTION('center_axis',(0.,0.,-1.));
#2787=DIRECTION('ref_axis',(1.,0.,0.));
#2788=DIRECTION('center_axis',(0.,0.,-1.));
#2789=DIRECTION('ref_axis',(1.,0.,0.));
#2790=DIRECTION('',(0.,0.,-1.));
#2791=DIRECTION('center_axis',(0.,0.,1.));
#2792=DIRECTION('ref_axis',(1.,0.,0.));
#2793=DIRECTION('center_axis',(0.,0.,-1.));
#2794=DIRECTION('ref_axis',(1.,0.,0.));
#2795=DIRECTION('center_axis',(0.,0.,-1.));
#2796=DIRECTION('ref_axis',(1.,0.,0.));
#2797=DIRECTION('',(0.,0.,-1.));
#2798=DIRECTION('center_axis',(0.,0.,1.));
#2799=DIRECTION('ref_axis',(1.,0.,0.));
#2800=DIRECTION('center_axis',(0.,1.,0.));
#2801=DIRECTION('ref_axis',(-1.,0.,0.));
#2802=DIRECTION('',(-1.,0.,0.));
#2803=DIRECTION('',(0.,0.,1.));
#2804=DIRECTION('',(-1.,0.,0.));
#2805=DIRECTION('',(0.,0.,1.));
#2806=DIRECTION('center_axis',(0.,0.,1.));
#2807=DIRECTION('ref_axis',(0.,-1.,0.));
#2808=DIRECTION('center_axis',(0.,0.,1.));
#2809=DIRECTION('ref_axis',(0.,-1.,0.));
#2810=DIRECTION('center_axis',(0.,0.,1.));
#2811=DIRECTION('ref_axis',(0.,-1.,0.));
#2812=DIRECTION('',(0.,0.,1.));
#2813=DIRECTION('center_axis',(0.,-1.,0.));
#2814=DIRECTION('ref_axis',(1.,0.,0.));
#2815=DIRECTION('',(1.,0.,0.));
#2816=DIRECTION('',(1.,0.,0.));
#2817=DIRECTION('',(0.,0.,1.));
#2818=DIRECTION('center_axis',(0.,0.,1.));
#2819=DIRECTION('ref_axis',(0.,1.,0.));
#2820=DIRECTION('center_axis',(0.,0.,1.));
#2821=DIRECTION('ref_axis',(0.,1.,0.));
#2822=DIRECTION('center_axis',(0.,0.,1.));
#2823=DIRECTION('ref_axis',(0.,1.,0.));
#2824=DIRECTION('center_axis',(0.,0.,1.));
#2825=DIRECTION('ref_axis',(1.,0.,0.));
#2826=DIRECTION('center_axis',(0.,0.,1.));
#2827=DIRECTION('ref_axis',(1.,0.,0.));
#2828=DIRECTION('axis',(0.,0.,1.));
#2829=DIRECTION('refdir',(1.,0.,0.));
#2830=DIRECTION('center_axis',(0.,0.,-1.));
#2831=DIRECTION('ref_axis',(1.,0.,0.));
#2832=DIRECTION('center_axis',(0.,0.,-1.));
#2833=DIRECTION('ref_axis',(1.,0.,0.));
#2834=DIRECTION('',(0.,0.,-1.));
#2835=DIRECTION('center_axis',(0.,0.,1.));
#2836=DIRECTION('ref_axis',(1.,0.,0.));
#2837=DIRECTION('center_axis',(0.,0.,-1.));
#2838=DIRECTION('ref_axis',(1.,0.,0.));
#2839=DIRECTION('center_axis',(0.,0.,-1.));
#2840=DIRECTION('ref_axis',(1.,0.,0.));
#2841=DIRECTION('',(0.,0.,-1.));
#2842=DIRECTION('center_axis',(0.,0.,1.));
#2843=DIRECTION('ref_axis',(1.,0.,0.));
#2844=DIRECTION('center_axis',(0.,1.,0.));
#2845=DIRECTION('ref_axis',(-1.,0.,0.));
#2846=DIRECTION('',(-1.,0.,0.));
#2847=DIRECTION('',(0.,0.,1.));
#2848=DIRECTION('',(-1.,0.,0.));
#2849=DIRECTION('',(0.,0.,1.));
#2850=DIRECTION('center_axis',(0.,0.,1.));
#2851=DIRECTION('ref_axis',(0.,-1.,0.));
#2852=DIRECTION('center_axis',(0.,0.,1.));
#2853=DIRECTION('ref_axis',(0.,-1.,0.));
#2854=DIRECTION('center_axis',(0.,0.,1.));
#2855=DIRECTION('ref_axis',(0.,-1.,0.));
#2856=DIRECTION('',(0.,0.,1.));
#2857=DIRECTION('center_axis',(0.,-1.,0.));
#2858=DIRECTION('ref_axis',(1.,0.,0.));
#2859=DIRECTION('',(1.,0.,0.));
#2860=DIRECTION('',(1.,0.,0.));
#2861=DIRECTION('',(0.,0.,1.));
#2862=DIRECTION('center_axis',(0.,0.,1.));
#2863=DIRECTION('ref_axis',(0.,1.,0.));
#2864=DIRECTION('center_axis',(0.,0.,1.));
#2865=DIRECTION('ref_axis',(0.,1.,0.));
#2866=DIRECTION('center_axis',(0.,0.,1.));
#2867=DIRECTION('ref_axis',(0.,1.,0.));
#2868=DIRECTION('center_axis',(0.,0.,1.));
#2869=DIRECTION('ref_axis',(1.,0.,0.));
#2870=DIRECTION('center_axis',(0.,0.,1.));
#2871=DIRECTION('ref_axis',(1.,0.,0.));
#2872=DIRECTION('axis',(0.,0.,1.));
#2873=DIRECTION('refdir',(1.,0.,0.));
#2874=DIRECTION('center_axis',(0.,0.,-1.));
#2875=DIRECTION('ref_axis',(1.,0.,0.));
#2876=DIRECTION('center_axis',(0.,0.,-1.));
#2877=DIRECTION('ref_axis',(1.,0.,0.));
#2878=DIRECTION('',(0.,0.,-1.));
#2879=DIRECTION('center_axis',(0.,0.,1.));
#2880=DIRECTION('ref_axis',(1.,0.,0.));
#2881=DIRECTION('center_axis',(0.,0.,-1.));
#2882=DIRECTION('ref_axis',(1.,0.,0.));
#2883=DIRECTION('center_axis',(0.,0.,-1.));
#2884=DIRECTION('ref_axis',(1.,0.,0.));
#2885=DIRECTION('',(0.,0.,-1.));
#2886=DIRECTION('center_axis',(0.,0.,1.));
#2887=DIRECTION('ref_axis',(1.,0.,0.));
#2888=DIRECTION('center_axis',(0.,0.,-1.));
#2889=DIRECTION('ref_axis',(1.,0.,0.));
#2890=DIRECTION('center_axis',(0.,0.,-1.));
#2891=DIRECTION('ref_axis',(1.,0.,0.));
#2892=DIRECTION('',(0.,0.,-1.));
#2893=DIRECTION('center_axis',(0.,0.,1.));
#2894=DIRECTION('ref_axis',(1.,0.,0.));
#2895=DIRECTION('center_axis',(0.,1.,0.));
#2896=DIRECTION('ref_axis',(-1.,0.,0.));
#2897=DIRECTION('',(-1.,0.,0.));
#2898=DIRECTION('',(0.,0.,1.));
#2899=DIRECTION('',(-1.,0.,0.));
#2900=DIRECTION('',(0.,0.,1.));
#2901=DIRECTION('center_axis',(0.,0.,1.));
#2902=DIRECTION('ref_axis',(0.,-1.,0.));
#2903=DIRECTION('center_axis',(0.,0.,1.));
#2904=DIRECTION('ref_axis',(0.,-1.,0.));
#2905=DIRECTION('center_axis',(0.,0.,1.));
#2906=DIRECTION('ref_axis',(0.,-1.,0.));
#2907=DIRECTION('',(0.,0.,1.));
#2908=DIRECTION('center_axis',(0.,-1.,0.));
#2909=DIRECTION('ref_axis',(1.,0.,0.));
#2910=DIRECTION('',(1.,0.,0.));
#2911=DIRECTION('',(1.,0.,0.));
#2912=DIRECTION('',(0.,0.,1.));
#2913=DIRECTION('center_axis',(0.,0.,1.));
#2914=DIRECTION('ref_axis',(0.,1.,0.));
#2915=DIRECTION('center_axis',(0.,0.,1.));
#2916=DIRECTION('ref_axis',(0.,1.,0.));
#2917=DIRECTION('center_axis',(0.,0.,1.));
#2918=DIRECTION('ref_axis',(0.,1.,0.));
#2919=DIRECTION('center_axis',(0.,0.,1.));
#2920=DIRECTION('ref_axis',(1.,0.,0.));
#2921=DIRECTION('center_axis',(0.,0.,1.));
#2922=DIRECTION('ref_axis',(1.,0.,0.));
#2923=DIRECTION('axis',(0.,0.,1.));
#2924=DIRECTION('refdir',(1.,0.,0.));
#2925=DIRECTION('center_axis',(0.,0.,-1.));
#2926=DIRECTION('ref_axis',(1.,0.,0.));
#2927=DIRECTION('center_axis',(0.,0.,-1.));
#2928=DIRECTION('ref_axis',(1.,0.,0.));
#2929=DIRECTION('',(0.,0.,-1.));
#2930=DIRECTION('center_axis',(0.,0.,1.));
#2931=DIRECTION('ref_axis',(1.,0.,0.));
#2932=DIRECTION('center_axis',(0.,0.,-1.));
#2933=DIRECTION('ref_axis',(1.,0.,0.));
#2934=DIRECTION('center_axis',(0.,0.,-1.));
#2935=DIRECTION('ref_axis',(1.,0.,0.));
#2936=DIRECTION('',(0.,0.,-1.));
#2937=DIRECTION('center_axis',(0.,0.,1.));
#2938=DIRECTION('ref_axis',(1.,0.,0.));
#2939=DIRECTION('center_axis',(0.,1.,0.));
#2940=DIRECTION('ref_axis',(-1.,0.,0.));
#2941=DIRECTION('',(-1.,0.,0.));
#2942=DIRECTION('',(0.,0.,1.));
#2943=DIRECTION('',(-1.,0.,0.));
#2944=DIRECTION('',(0.,0.,1.));
#2945=DIRECTION('center_axis',(0.,0.,1.));
#2946=DIRECTION('ref_axis',(0.,-1.,0.));
#2947=DIRECTION('center_axis',(0.,0.,1.));
#2948=DIRECTION('ref_axis',(0.,-1.,0.));
#2949=DIRECTION('center_axis',(0.,0.,1.));
#2950=DIRECTION('ref_axis',(0.,-1.,0.));
#2951=DIRECTION('',(0.,0.,1.));
#2952=DIRECTION('center_axis',(0.,-1.,0.));
#2953=DIRECTION('ref_axis',(1.,0.,0.));
#2954=DIRECTION('',(1.,0.,0.));
#2955=DIRECTION('',(1.,0.,0.));
#2956=DIRECTION('',(0.,0.,1.));
#2957=DIRECTION('center_axis',(0.,0.,1.));
#2958=DIRECTION('ref_axis',(0.,1.,0.));
#2959=DIRECTION('center_axis',(0.,0.,1.));
#2960=DIRECTION('ref_axis',(0.,1.,0.));
#2961=DIRECTION('center_axis',(0.,0.,1.));
#2962=DIRECTION('ref_axis',(0.,1.,0.));
#2963=DIRECTION('center_axis',(0.,0.,1.));
#2964=DIRECTION('ref_axis',(1.,0.,0.));
#2965=DIRECTION('center_axis',(0.,0.,1.));
#2966=DIRECTION('ref_axis',(1.,0.,0.));
#2967=DIRECTION('axis',(0.,0.,1.));
#2968=DIRECTION('refdir',(1.,0.,0.));
#2969=DIRECTION('center_axis',(0.,0.,-1.));
#2970=DIRECTION('ref_axis',(1.,0.,0.));
#2971=DIRECTION('center_axis',(0.,0.,-1.));
#2972=DIRECTION('ref_axis',(1.,0.,0.));
#2973=DIRECTION('',(0.,0.,-1.));
#2974=DIRECTION('center_axis',(0.,0.,1.));
#2975=DIRECTION('ref_axis',(1.,0.,0.));
#2976=DIRECTION('center_axis',(0.,0.,-1.));
#2977=DIRECTION('ref_axis',(1.,0.,0.));
#2978=DIRECTION('center_axis',(0.,0.,-1.));
#2979=DIRECTION('ref_axis',(1.,0.,0.));
#2980=DIRECTION('',(0.,0.,-1.));
#2981=DIRECTION('center_axis',(0.,0.,1.));
#2982=DIRECTION('ref_axis',(1.,0.,0.));
#2983=DIRECTION('center_axis',(0.,1.,0.));
#2984=DIRECTION('ref_axis',(-1.,0.,0.));
#2985=DIRECTION('',(-1.,0.,0.));
#2986=DIRECTION('',(0.,0.,1.));
#2987=DIRECTION('',(-1.,0.,0.));
#2988=DIRECTION('',(0.,0.,1.));
#2989=DIRECTION('center_axis',(0.,0.,1.));
#2990=DIRECTION('ref_axis',(0.,-1.,0.));
#2991=DIRECTION('center_axis',(0.,0.,1.));
#2992=DIRECTION('ref_axis',(0.,-1.,0.));
#2993=DIRECTION('center_axis',(0.,0.,1.));
#2994=DIRECTION('ref_axis',(0.,-1.,0.));
#2995=DIRECTION('',(0.,0.,1.));
#2996=DIRECTION('center_axis',(0.,-1.,0.));
#2997=DIRECTION('ref_axis',(1.,0.,0.));
#2998=DIRECTION('',(1.,0.,0.));
#2999=DIRECTION('',(1.,0.,0.));
#3000=DIRECTION('',(0.,0.,1.));
#3001=DIRECTION('center_axis',(0.,0.,1.));
#3002=DIRECTION('ref_axis',(0.,1.,0.));
#3003=DIRECTION('center_axis',(0.,0.,1.));
#3004=DIRECTION('ref_axis',(0.,1.,0.));
#3005=DIRECTION('center_axis',(0.,0.,1.));
#3006=DIRECTION('ref_axis',(0.,1.,0.));
#3007=DIRECTION('center_axis',(0.,0.,1.));
#3008=DIRECTION('ref_axis',(1.,0.,0.));
#3009=DIRECTION('center_axis',(0.,0.,1.));
#3010=DIRECTION('ref_axis',(1.,0.,0.));
#3011=DIRECTION('axis',(0.,0.,1.));
#3012=DIRECTION('refdir',(1.,0.,0.));
#3013=DIRECTION('center_axis',(0.,0.,1.));
#3014=DIRECTION('ref_axis',(1.,0.,0.));
#3015=DIRECTION('center_axis',(0.,0.,1.));
#3016=DIRECTION('ref_axis',(1.,0.,0.));
#3017=DIRECTION('',(0.,0.,-1.));
#3018=DIRECTION('center_axis',(0.,0.,1.));
#3019=DIRECTION('ref_axis',(1.,0.,0.));
#3020=DIRECTION('center_axis',(0.,0.,1.));
#3021=DIRECTION('ref_axis',(1.,0.,0.));
#3022=DIRECTION('center_axis',(0.,0.,1.));
#3023=DIRECTION('ref_axis',(1.,0.,0.));
#3024=DIRECTION('axis',(0.,0.,1.));
#3025=DIRECTION('refdir',(1.,0.,0.));
#3026=DIRECTION('center_axis',(0.,0.,1.));
#3027=DIRECTION('ref_axis',(1.,0.,0.));
#3028=DIRECTION('center_axis',(0.,0.,-1.));
#3029=DIRECTION('ref_axis',(1.,0.,0.));
#3030=DIRECTION('',(0.,0.,-1.));
#3031=DIRECTION('center_axis',(0.,0.,-1.));
#3032=DIRECTION('ref_axis',(1.,0.,0.));
#3033=DIRECTION('center_axis',(0.,0.,1.));
#3034=DIRECTION('ref_axis',(1.,0.,0.));
#3035=DIRECTION('center_axis',(0.,0.,1.));
#3036=DIRECTION('ref_axis',(1.,0.,0.));
#3037=DIRECTION('',(0.,0.,-1.));
#3038=DIRECTION('center_axis',(0.,0.,1.));
#3039=DIRECTION('ref_axis',(1.,0.,0.));
#3040=DIRECTION('center_axis',(0.,0.,1.));
#3041=DIRECTION('ref_axis',(1.,0.,0.));
#3042=DIRECTION('center_axis',(0.,0.,1.));
#3043=DIRECTION('ref_axis',(1.,0.,0.));
#3044=DIRECTION('axis',(0.,0.,1.));
#3045=DIRECTION('refdir',(1.,0.,0.));
#3046=DIRECTION('center_axis',(0.,0.,1.));
#3047=DIRECTION('ref_axis',(1.,0.,0.));
#3048=DIRECTION('center_axis',(0.,0.,1.));
#3049=DIRECTION('ref_axis',(1.,0.,0.));
#3050=DIRECTION('',(0.,0.,1.));
#3051=DIRECTION('center_axis',(0.,0.,1.));
#3052=DIRECTION('ref_axis',(1.,0.,0.));
#3053=DIRECTION('center_axis',(0.,0.,-1.));
#3054=DIRECTION('ref_axis',(-1.,0.,0.));
#3055=DIRECTION('center_axis',(0.,0.,-1.));
#3056=DIRECTION('ref_axis',(1.,0.,0.));
#3057=DIRECTION('center_axis',(0.,0.,1.));
#3058=DIRECTION('ref_axis',(1.,0.,0.));
#3059=DIRECTION('center_axis',(0.,0.,1.));
#3060=DIRECTION('ref_axis',(1.,0.,0.));
#3061=DIRECTION('center_axis',(0.,0.,1.));
#3062=DIRECTION('ref_axis',(1.,0.,0.));
#3063=DIRECTION('center_axis',(0.,0.,1.));
#3064=DIRECTION('ref_axis',(1.,0.,0.));
#3065=DIRECTION('',(0.,0.,-1.));
#3066=DIRECTION('center_axis',(0.,0.,1.));
#3067=DIRECTION('ref_axis',(1.,0.,0.));
#3068=DIRECTION('center_axis',(0.,0.,1.));
#3069=DIRECTION('ref_axis',(1.,0.,0.));
#3070=DIRECTION('center_axis',(0.,0.,1.));
#3071=DIRECTION('ref_axis',(1.,0.,0.));
#3072=DIRECTION('center_axis',(0.,0.,1.));
#3073=DIRECTION('ref_axis',(1.,0.,0.));
#3074=DIRECTION('',(0.,0.,-1.));
#3075=DIRECTION('center_axis',(0.,0.,1.));
#3076=DIRECTION('ref_axis',(1.,0.,0.));
#3077=DIRECTION('center_axis',(0.,0.,1.));
#3078=DIRECTION('ref_axis',(1.,0.,0.));
#3079=DIRECTION('center_axis',(0.,0.,1.));
#3080=DIRECTION('ref_axis',(1.,0.,0.));
#3081=DIRECTION('',(0.,0.,-1.));
#3082=DIRECTION('center_axis',(0.,0.,1.));
#3083=DIRECTION('ref_axis',(1.,0.,0.));
#3084=DIRECTION('axis',(0.,0.,1.));
#3085=DIRECTION('refdir',(1.,0.,0.));
#3086=DIRECTION('center_axis',(0.,0.,1.));
#3087=DIRECTION('ref_axis',(1.,0.,0.));
#3088=DIRECTION('center_axis',(0.,0.,-1.));
#3089=DIRECTION('ref_axis',(1.,0.,0.));
#3090=DIRECTION('',(0.707106781186547,8.65956056235493E-17,-0.707106781186548));
#3091=DIRECTION('center_axis',(0.,0.,1.));
#3092=DIRECTION('ref_axis',(1.,0.,0.));
#3093=DIRECTION('center_axis',(0.,0.,1.));
#3094=DIRECTION('ref_axis',(1.,0.,0.));
#3095=DIRECTION('center_axis',(0.,0.,1.));
#3096=DIRECTION('ref_axis',(1.,0.,0.));
#3097=DIRECTION('',(0.,0.,-1.));
#3098=DIRECTION('center_axis',(0.,0.,1.));
#3099=DIRECTION('ref_axis',(1.,0.,0.));
#3100=DIRECTION('center_axis',(0.,0.,-1.));
#3101=DIRECTION('ref_axis',(1.,0.,0.));
#3102=DIRECTION('center_axis',(0.,0.,-1.));
#3103=DIRECTION('ref_axis',(1.,0.,0.));
#3104=DIRECTION('center_axis',(0.,0.,-1.));
#3105=DIRECTION('ref_axis',(1.,0.,0.));
#3106=DIRECTION('',(-0.707106781186548,-8.65956056235493E-17,-0.707106781186548));
#3107=DIRECTION('center_axis',(0.,0.,1.));
#3108=DIRECTION('ref_axis',(1.,0.,0.));
#3109=DIRECTION('center_axis',(0.,0.,1.));
#3110=DIRECTION('ref_axis',(1.,0.,0.));
#3111=DIRECTION('center_axis',(0.,0.,-1.));
#3112=DIRECTION('ref_axis',(1.,0.,0.));
#3113=DIRECTION('center_axis',(0.,0.,1.));
#3114=DIRECTION('ref_axis',(1.,0.,0.));
#3115=DIRECTION('',(-0.707106781186547,-8.65956056235493E-17,-0.707106781186548));
#3116=DIRECTION('center_axis',(0.,0.,1.));
#3117=DIRECTION('ref_axis',(1.,0.,0.));
#3118=DIRECTION('center_axis',(0.,0.,-1.));
#3119=DIRECTION('ref_axis',(1.,0.,0.));
#3120=DIRECTION('',(0.,0.,-1.));
#3121=DIRECTION('center_axis',(0.,0.,1.));
#3122=DIRECTION('ref_axis',(1.,0.,0.));
#3123=DIRECTION('',(0.707106781186548,8.65956056235493E-17,-0.707106781186548));
#3124=DIRECTION('axis',(0.,0.,1.));
#3125=DIRECTION('refdir',(1.,0.,0.));
#3126=DIRECTION('center_axis',(0.,0.,1.));
#3127=DIRECTION('ref_axis',(1.,0.,0.));
#3128=DIRECTION('center_axis',(0.,0.,-1.));
#3129=DIRECTION('ref_axis',(1.,0.,0.));
#3130=DIRECTION('',(0.,0.,-1.));
#3131=DIRECTION('center_axis',(0.,0.,-1.));
#3132=DIRECTION('ref_axis',(1.,0.,0.));
#3133=DIRECTION('center_axis',(0.,0.,1.));
#3134=DIRECTION('ref_axis',(1.,0.,0.));
#3135=DIRECTION('center_axis',(0.,0.,1.));
#3136=DIRECTION('ref_axis',(1.,0.,0.));
#3137=DIRECTION('',(0.,0.,-1.));
#3138=DIRECTION('center_axis',(0.,0.,1.));
#3139=DIRECTION('ref_axis',(1.,0.,0.));
#3140=DIRECTION('center_axis',(0.,0.,1.));
#3141=DIRECTION('ref_axis',(1.,0.,0.));
#3142=DIRECTION('center_axis',(0.,0.,1.));
#3143=DIRECTION('ref_axis',(1.,0.,0.));
#3144=DIRECTION('axis',(0.,0.,1.));
#3145=DIRECTION('refdir',(1.,0.,0.));
#3146=DIRECTION('center_axis',(0.,0.,1.));
#3147=DIRECTION('ref_axis',(1.,0.,0.));
#3148=DIRECTION('center_axis',(0.,0.,1.));
#3149=DIRECTION('ref_axis',(1.,0.,0.));
#3150=DIRECTION('',(0.,0.,1.));
#3151=DIRECTION('center_axis',(0.,0.,1.));
#3152=DIRECTION('ref_axis',(1.,0.,0.));
#3153=DIRECTION('center_axis',(0.,0.,-1.));
#3154=DIRECTION('ref_axis',(-1.,0.,0.));
#3155=DIRECTION('center_axis',(0.,0.,-1.));
#3156=DIRECTION('ref_axis',(1.,0.,0.));
#3157=DIRECTION('center_axis',(0.,0.,1.));
#3158=DIRECTION('ref_axis',(1.,0.,0.));
#3159=DIRECTION('center_axis',(0.,0.,1.));
#3160=DIRECTION('ref_axis',(1.,0.,0.));
#3161=DIRECTION('center_axis',(0.,0.,1.));
#3162=DIRECTION('ref_axis',(1.,0.,0.));
#3163=DIRECTION('center_axis',(0.,0.,1.));
#3164=DIRECTION('ref_axis',(1.,0.,0.));
#3165=DIRECTION('',(0.,0.,-1.));
#3166=DIRECTION('center_axis',(0.,0.,1.));
#3167=DIRECTION('ref_axis',(1.,0.,0.));
#3168=DIRECTION('center_axis',(0.,0.,1.));
#3169=DIRECTION('ref_axis',(1.,0.,0.));
#3170=DIRECTION('center_axis',(0.,0.,1.));
#3171=DIRECTION('ref_axis',(1.,0.,0.));
#3172=DIRECTION('center_axis',(0.,0.,1.));
#3173=DIRECTION('ref_axis',(1.,0.,0.));
#3174=DIRECTION('',(0.,0.,-1.));
#3175=DIRECTION('center_axis',(0.,0.,1.));
#3176=DIRECTION('ref_axis',(1.,0.,0.));
#3177=DIRECTION('center_axis',(0.,0.,1.));
#3178=DIRECTION('ref_axis',(1.,0.,0.));
#3179=DIRECTION('center_axis',(0.,0.,1.));
#3180=DIRECTION('ref_axis',(1.,0.,0.));
#3181=DIRECTION('',(0.,0.,-1.));
#3182=DIRECTION('center_axis',(0.,0.,1.));
#3183=DIRECTION('ref_axis',(1.,0.,0.));
#3184=DIRECTION('axis',(0.,0.,1.));
#3185=DIRECTION('refdir',(1.,0.,0.));
#3186=DIRECTION('center_axis',(0.,0.,1.));
#3187=DIRECTION('ref_axis',(1.,0.,0.));
#3188=DIRECTION('center_axis',(0.,0.,-1.));
#3189=DIRECTION('ref_axis',(1.,0.,0.));
#3190=DIRECTION('',(0.,0.,-1.));
#3191=DIRECTION('center_axis',(0.,0.,-1.));
#3192=DIRECTION('ref_axis',(1.,0.,0.));
#3193=DIRECTION('center_axis',(0.,0.,1.));
#3194=DIRECTION('ref_axis',(1.,0.,0.));
#3195=DIRECTION('center_axis',(0.,0.,1.));
#3196=DIRECTION('ref_axis',(1.,0.,0.));
#3197=DIRECTION('',(0.,0.,-1.));
#3198=DIRECTION('center_axis',(0.,0.,1.));
#3199=DIRECTION('ref_axis',(1.,0.,0.));
#3200=DIRECTION('center_axis',(0.,0.,1.));
#3201=DIRECTION('ref_axis',(1.,0.,0.));
#3202=DIRECTION('center_axis',(0.,0.,1.));
#3203=DIRECTION('ref_axis',(1.,0.,0.));
#3204=DIRECTION('axis',(0.,0.,1.));
#3205=DIRECTION('refdir',(1.,0.,0.));
#3206=DIRECTION('center_axis',(-1.,0.,0.));
#3207=DIRECTION('ref_axis',(0.,1.,0.));
#3208=DIRECTION('',(0.,0.,1.));
#3209=DIRECTION('',(0.,-1.,0.));
#3210=DIRECTION('',(0.,0.,-1.));
#3211=DIRECTION('',(0.,1.,0.));
#3212=DIRECTION('center_axis',(1.,0.,0.));
#3213=DIRECTION('ref_axis',(0.,-1.,0.));
#3214=DIRECTION('',(0.,0.,-1.));
#3215=DIRECTION('',(0.,-1.,0.));
#3216=DIRECTION('',(0.,0.,1.));
#3217=DIRECTION('',(0.,1.,0.));
#3218=DIRECTION('center_axis',(0.,0.,1.));
#3219=DIRECTION('ref_axis',(1.,0.,0.));
#3220=DIRECTION('center_axis',(0.,0.,1.));
#3221=DIRECTION('ref_axis',(1.,0.,0.));
#3222=DIRECTION('center_axis',(0.,0.,-1.));
#3223=DIRECTION('ref_axis',(1.,0.,0.));
#3224=DIRECTION('center_axis',(0.,0.,1.));
#3225=DIRECTION('ref_axis',(6.12323399573677E-17,-1.,0.));
#3226=DIRECTION('center_axis',(0.,0.,-1.));
#3227=DIRECTION('ref_axis',(1.,0.,0.));
#3228=DIRECTION('center_axis',(0.,0.,1.));
#3229=DIRECTION('ref_axis',(6.12323399573677E-17,-1.,0.));
#3230=DIRECTION('center_axis',(0.,0.,1.));
#3231=DIRECTION('ref_axis',(1.,0.,0.));
#3232=DIRECTION('center_axis',(0.,0.,1.));
#3233=DIRECTION('ref_axis',(1.,0.,0.));
#3234=DIRECTION('axis',(0.,0.,1.));
#3235=DIRECTION('refdir',(1.,0.,0.));
#3236=DIRECTION('center_axis',(0.,0.,1.));
#3237=DIRECTION('ref_axis',(1.,0.,0.));
#3238=DIRECTION('center_axis',(0.,0.,1.));
#3239=DIRECTION('ref_axis',(1.,0.,0.));
#3240=DIRECTION('',(0.,0.,1.));
#3241=DIRECTION('center_axis',(0.,0.,1.));
#3242=DIRECTION('ref_axis',(1.,0.,0.));
#3243=DIRECTION('center_axis',(0.,0.,-1.));
#3244=DIRECTION('ref_axis',(-1.,0.,0.));
#3245=DIRECTION('center_axis',(0.,0.,-1.));
#3246=DIRECTION('ref_axis',(1.,0.,0.));
#3247=DIRECTION('center_axis',(0.,0.,1.));
#3248=DIRECTION('ref_axis',(1.,0.,0.));
#3249=DIRECTION('center_axis',(0.,0.,1.));
#3250=DIRECTION('ref_axis',(1.,0.,0.));
#3251=DIRECTION('center_axis',(0.,0.,1.));
#3252=DIRECTION('ref_axis',(1.,0.,0.));
#3253=DIRECTION('center_axis',(0.,0.,1.));
#3254=DIRECTION('ref_axis',(1.,0.,0.));
#3255=DIRECTION('',(0.,0.,-1.));
#3256=DIRECTION('center_axis',(0.,0.,1.));
#3257=DIRECTION('ref_axis',(1.,0.,0.));
#3258=DIRECTION('center_axis',(0.,0.,1.));
#3259=DIRECTION('ref_axis',(1.,0.,0.));
#3260=DIRECTION('center_axis',(0.,0.,1.));
#3261=DIRECTION('ref_axis',(1.,0.,0.));
#3262=DIRECTION('center_axis',(0.,0.,1.));
#3263=DIRECTION('ref_axis',(1.,0.,0.));
#3264=DIRECTION('',(0.,0.,-1.));
#3265=DIRECTION('center_axis',(0.,0.,1.));
#3266=DIRECTION('ref_axis',(1.,0.,0.));
#3267=DIRECTION('center_axis',(0.,0.,1.));
#3268=DIRECTION('ref_axis',(1.,0.,0.));
#3269=DIRECTION('center_axis',(0.,0.,1.));
#3270=DIRECTION('ref_axis',(1.,0.,0.));
#3271=DIRECTION('',(0.,0.,-1.));
#3272=DIRECTION('center_axis',(0.,0.,1.));
#3273=DIRECTION('ref_axis',(1.,0.,0.));
#3274=DIRECTION('axis',(0.,0.,1.));
#3275=DIRECTION('refdir',(1.,0.,0.));
#3276=DIRECTION('center_axis',(0.,0.,1.));
#3277=DIRECTION('ref_axis',(1.,0.,0.));
#3278=DIRECTION('center_axis',(0.,0.,-1.));
#3279=DIRECTION('ref_axis',(1.,0.,0.));
#3280=DIRECTION('',(0.,0.,-1.));
#3281=DIRECTION('center_axis',(0.,0.,-1.));
#3282=DIRECTION('ref_axis',(1.,0.,0.));
#3283=DIRECTION('center_axis',(0.,0.,1.));
#3284=DIRECTION('ref_axis',(1.,0.,0.));
#3285=DIRECTION('center_axis',(0.,0.,1.));
#3286=DIRECTION('ref_axis',(1.,0.,0.));
#3287=DIRECTION('',(0.,0.,-1.));
#3288=DIRECTION('center_axis',(0.,0.,1.));
#3289=DIRECTION('ref_axis',(1.,0.,0.));
#3290=DIRECTION('center_axis',(0.,0.,1.));
#3291=DIRECTION('ref_axis',(1.,0.,0.));
#3292=DIRECTION('center_axis',(0.,0.,1.));
#3293=DIRECTION('ref_axis',(1.,0.,0.));
#3294=DIRECTION('axis',(0.,0.,1.));
#3295=DIRECTION('refdir',(1.,0.,0.));
#3296=DIRECTION('center_axis',(0.,0.,1.));
#3297=DIRECTION('ref_axis',(1.,0.,0.));
#3298=DIRECTION('center_axis',(0.,0.,-1.));
#3299=DIRECTION('ref_axis',(1.,0.,0.));
#3300=DIRECTION('',(0.,0.,-1.));
#3301=DIRECTION('center_axis',(0.,0.,-1.));
#3302=DIRECTION('ref_axis',(1.,0.,0.));
#3303=DIRECTION('center_axis',(0.,0.,1.));
#3304=DIRECTION('ref_axis',(1.,0.,0.));
#3305=DIRECTION('center_axis',(0.,0.,1.));
#3306=DIRECTION('ref_axis',(1.,0.,0.));
#3307=DIRECTION('',(0.,0.,-1.));
#3308=DIRECTION('center_axis',(0.,0.,1.));
#3309=DIRECTION('ref_axis',(1.,0.,0.));
#3310=DIRECTION('center_axis',(0.,0.,1.));
#3311=DIRECTION('ref_axis',(1.,0.,0.));
#3312=DIRECTION('center_axis',(0.,0.,1.));
#3313=DIRECTION('ref_axis',(1.,0.,0.));
#3314=DIRECTION('',(0.,0.,1.));
#3315=DIRECTION('',(1.,0.,0.));
#3316=DIRECTION('',(0.,-1.,0.));
#3317=DIRECTION('',(1.,0.,0.));
#3318=DIRECTION('',(6.12323399651827E-17,-1.,6.12323399354591E-17));
#3319=DIRECTION('',(0.388778686861485,8.02210923798446E-17,0.921331174248583));
#3320=DIRECTION('',(6.12323399520215E-17,-1.,6.12323399621973E-17));
#3321=DIRECTION('',(0.294584799207545,7.65532924453796E-17,0.95562534294349));
#3322=DIRECTION('',(2.51425407660377E-17,-1.,1.22055727365509E-16));
#3323=DIRECTION('',(0.873743927690279,8.1334365408083E-17,0.486386213645471));
#3324=DIRECTION('',(6.1232339955146E-17,-1.,6.1232339959571E-17));
#3325=DIRECTION('',(0.244648308183105,-4.43912161246229E-17,-0.969611883850006));
#3326=DIRECTION('',(1.22514472112306E-19,-1.,3.02672766688838E-17));
#3327=DIRECTION('',(-0.309050343414937,-2.88234258576189E-17,-0.951045679888785));
#3328=DIRECTION('',(1.22514472112278E-19,-1.,3.02672766688838E-17));
#3329=DIRECTION('',(0.983514536213433,-5.35270910384196E-18,-0.180829082442196));
#3330=DIRECTION('',(6.12323399651827E-17,-1.,6.12323399354591E-17));
#3331=DIRECTION('',(0.388778686861485,8.02210923798446E-17,0.921331174248583));
#3332=DIRECTION('',(0.,-1.,0.));
#3333=DIRECTION('',(1.,0.,0.));
#3334=DIRECTION('',(0.,-1.,0.));
#3335=DIRECTION('',(1.,0.,0.));
#3336=DIRECTION('',(6.12323399651827E-17,-1.,6.12323399354591E-17));
#3337=DIRECTION('',(0.388778686861485,8.02210923798446E-17,0.921331174248583));
#3338=DIRECTION('',(6.12323399520214E-17,-1.,6.12323399621973E-17));
#3339=DIRECTION('',(0.998926459410359,5.83300672477601E-17,-0.0463241696082971));
#3340=DIRECTION('',(6.12323399520214E-17,-1.,6.12323399621973E-17));
#3341=DIRECTION('',(0.998926459410359,5.83300672477601E-17,-0.0463241696082971));
#3342=DIRECTION('',(2.51425407660377E-17,-1.,1.22055727365509E-16));
#3343=DIRECTION('',(0.953905020025902,-1.26463859411783E-17,-0.300108668267671));
#3344=DIRECTION('',(2.51425407660377E-17,-1.,1.22055727365509E-16));
#3345=DIRECTION('',(0.953905020025902,-1.26463859411783E-17,-0.300108668267671));
#3346=DIRECTION('',(2.51425407660377E-17,-1.,1.22055727365509E-16));
#3347=DIRECTION('',(0.953905020025902,-1.26463859411783E-17,-0.300108668267671));
#3348=DIRECTION('',(6.1232339955146E-17,-1.,6.1232339959571E-17));
#3349=DIRECTION('',(0.991758766002538,5.28826665693203E-17,-0.128119280583122));
#3350=DIRECTION('',(6.1232339955146E-17,-1.,6.1232339959571E-17));
#3351=DIRECTION('',(0.991758766002538,5.28826665693203E-17,-0.128119280583122));
#3352=DIRECTION('',(1.22514472112277E-19,-1.,3.02672766688838E-17));
#3353=DIRECTION('',(0.983514536213433,-5.35270910384189E-18,-0.180829082442196));
#3354=DIRECTION('',(1.22514472112204E-19,-1.,3.02672766688838E-17));
#3355=DIRECTION('',(0.983514536213433,-5.35270910384189E-18,-0.180829082442196));
#3356=DIRECTION('',(0.,-1.,0.));
#3357=DIRECTION('',(1.,0.,0.));
#3358=DIRECTION('',(0.,1.,-1.22464679914735E-16));
#3359=DIRECTION('',(1.,0.,0.));
#3360=DIRECTION('',(0.,-1.,0.));
#3361=DIRECTION('',(1.,0.,0.));
#3362=DIRECTION('',(0.,-1.,0.));
#3363=DIRECTION('',(1.,0.,0.));
#3364=DIRECTION('',(0.,1.,-1.22464679914735E-16));
#3365=DIRECTION('',(1.,0.,0.));
#3366=DIRECTION('',(0.,-1.,0.));
#3367=DIRECTION('',(1.,0.,0.));
#3368=DIRECTION('',(0.,-1.,0.));
#3369=DIRECTION('',(1.,0.,0.));
#3370=DIRECTION('',(0.,1.,-1.22464679914735E-16));
#3371=DIRECTION('',(1.,0.,0.));
#3372=DIRECTION('',(6.12323399651827E-17,-1.,6.12323399354591E-17));
#3373=DIRECTION('',(0.388778686861485,8.02210923798446E-17,0.921331174248583));
#3374=DIRECTION('',(6.12323399520214E-17,-1.,6.12323399621973E-17));
#3375=DIRECTION('',(0.998926459410359,5.83300672477601E-17,-0.0463241696082971));
#3376=DIRECTION('',(2.51425407660377E-17,-1.,1.22055727365509E-16));
#3377=DIRECTION('',(0.953905020025902,-1.26463859411783E-17,-0.300108668267671));
#3378=DIRECTION('',(6.1232339955146E-17,-1.,6.1232339959571E-17));
#3379=DIRECTION('',(0.991758766002538,5.28826665693203E-17,-0.128119280583122));
#3380=DIRECTION('',(6.12323399651827E-17,-1.,6.12323399354591E-17));
#3381=DIRECTION('',(0.388778686861485,8.02210923798446E-17,0.921331174248583));
#3382=DIRECTION('',(6.1232339955146E-17,-1.,6.1232339959571E-17));
#3383=DIRECTION('',(0.991758766002538,5.28826665693203E-17,-0.128119280583122));
#3384=DIRECTION('',(6.12323399651827E-17,-1.,6.12323399354591E-17));
#3385=DIRECTION('',(0.388778686861485,8.02210923798446E-17,0.921331174248583));
#3386=DIRECTION('',(6.12323399651826E-17,-1.,6.12323399354591E-17));
#3387=DIRECTION('',(0.388778686861485,8.02210923798446E-17,0.921331174248583));
#3388=DIRECTION('',(6.1232339955146E-17,-1.,6.1232339959571E-17));
#3389=DIRECTION('',(0.991758766002538,5.28826665693203E-17,-0.128119280583122));
#3390=DIRECTION('',(0.,-1.,0.));
#3391=DIRECTION('',(1.,0.,0.));
#3392=DIRECTION('',(0.,1.,-1.22464679914735E-16));
#3393=DIRECTION('',(1.,0.,0.));
#3394=DIRECTION('',(6.12323399651827E-17,-1.,6.12323399354591E-17));
#3395=DIRECTION('',(0.388778686861485,8.02210923798446E-17,0.921331174248583));
#3396=DIRECTION('',(6.12323399520214E-17,-1.,6.12323399621973E-17));
#3397=DIRECTION('',(0.998926459410359,5.83300672477601E-17,-0.0463241696082971));
#3398=DIRECTION('',(2.51425407660377E-17,-1.,1.22055727365509E-16));
#3399=DIRECTION('',(0.953905020025902,-1.26463859411783E-17,-0.300108668267671));
#3400=DIRECTION('',(6.1232339955146E-17,-1.,6.1232339959571E-17));
#3401=DIRECTION('',(0.991758766002538,5.28826665693203E-17,-0.128119280583122));
#3402=DIRECTION('',(6.12323399520214E-17,-1.,6.12323399621973E-17));
#3403=DIRECTION('',(0.998926459410359,5.83300672477601E-17,-0.0463241696082971));
#3404=DIRECTION('',(2.51425407660377E-17,-1.,1.22055727365509E-16));
#3405=DIRECTION('',(0.953905020025902,-1.26463859411783E-17,-0.300108668267671));
#3406=DIRECTION('',(6.12323399520214E-17,-1.,6.12323399621973E-17));
#3407=DIRECTION('',(0.998926459410359,5.833006724776E-17,-0.0463241696082971));
#3408=DIRECTION('',(2.51425407660378E-17,-1.,1.22055727365509E-16));
#3409=DIRECTION('',(0.953905020025902,-1.26463859411783E-17,-0.300108668267671));
#3410=DIRECTION('',(6.1232339955146E-17,-1.,6.1232339959571E-17));
#3411=DIRECTION('',(0.991758766002538,5.28826665693203E-17,-0.128119280583122));
#3412=DIRECTION('',(6.12323399520215E-17,-1.,6.12323399621973E-17));
#3413=DIRECTION('',(0.998926459410359,5.833006724776E-17,-0.0463241696082971));
#3414=DIRECTION('',(2.51425407660378E-17,-1.,1.22055727365509E-16));
#3415=DIRECTION('',(0.953905020025902,-1.26463859411783E-17,-0.300108668267671));
#3416=CARTESIAN_POINT('',(0.,0.,0.));
#3417=CARTESIAN_POINT('',(0.,0.,0.));
#3418=CARTESIAN_POINT('Origin',(170.,-90.,6.));
#3419=CARTESIAN_POINT('',(165.5,-90.,12.));
#3420=CARTESIAN_POINT('Origin',(170.,-90.,12.));
#3421=CARTESIAN_POINT('',(165.5,-90.,-5.));
#3422=CARTESIAN_POINT('',(165.5,-90.,6.));
#3423=CARTESIAN_POINT('Origin',(170.,-90.,-5.));
#3424=CARTESIAN_POINT('Origin',(-50.,-90.,6.));
#3425=CARTESIAN_POINT('',(-54.5,-90.,12.));
#3426=CARTESIAN_POINT('Origin',(-50.,-90.,12.));
#3427=CARTESIAN_POINT('',(-54.5,-90.,-5.));
#3428=CARTESIAN_POINT('',(-54.5,-90.,6.));
#3429=CARTESIAN_POINT('Origin',(-50.,-90.,-5.));
#3430=CARTESIAN_POINT('Origin',(-50.,30.,6.));
#3431=CARTESIAN_POINT('',(-54.5,30.,12.));
#3432=CARTESIAN_POINT('Origin',(-50.,30.,12.));
#3433=CARTESIAN_POINT('',(-54.5,30.,-5.));
#3434=CARTESIAN_POINT('',(-54.5,30.,6.));
#3435=CARTESIAN_POINT('Origin',(-50.,30.,-5.));
#3436=CARTESIAN_POINT('Origin',(170.,30.,6.));
#3437=CARTESIAN_POINT('',(165.5,30.,12.));
#3438=CARTESIAN_POINT('Origin',(170.,30.,12.));
#3439=CARTESIAN_POINT('',(165.5,30.,-5.));
#3440=CARTESIAN_POINT('',(165.5,30.,6.));
#3441=CARTESIAN_POINT('Origin',(170.,30.,-5.));
#3442=CARTESIAN_POINT('Origin',(190.,55.,0.));
#3443=CARTESIAN_POINT('',(195.,55.,-5.));
#3444=CARTESIAN_POINT('',(-75.,55.,-5.));
#3445=CARTESIAN_POINT('',(125.,55.,-5.));
#3446=CARTESIAN_POINT('',(-75.,55.,12.));
#3447=CARTESIAN_POINT('',(-75.,55.,0.));
#3448=CARTESIAN_POINT('',(195.,55.,12.));
#3449=CARTESIAN_POINT('',(125.,55.,12.));
#3450=CARTESIAN_POINT('',(195.,55.,0.));
#3451=CARTESIAN_POINT('Origin',(195.,-110.,0.));
#3452=CARTESIAN_POINT('',(195.,-115.,-5.));
#3453=CARTESIAN_POINT('',(195.,-70.,-5.));
#3454=CARTESIAN_POINT('',(195.,-115.,12.));
#3455=CARTESIAN_POINT('',(195.,-70.,12.));
#3456=CARTESIAN_POINT('',(195.,-115.,0.));
#3457=CARTESIAN_POINT('Origin',(-70.,-115.,0.));
#3458=CARTESIAN_POINT('',(-75.,-115.,-5.));
#3459=CARTESIAN_POINT('',(-5.,-115.,-5.));
#3460=CARTESIAN_POINT('',(-75.,-115.,12.));
#3461=CARTESIAN_POINT('',(-5.,-115.,12.));
#3462=CARTESIAN_POINT('',(-75.,-115.,0.));
#3463=CARTESIAN_POINT('Origin',(-75.,50.,0.));
#3464=CARTESIAN_POINT('',(-75.,10.,-5.));
#3465=CARTESIAN_POINT('',(-75.,10.,12.));
#3466=CARTESIAN_POINT('Origin',(60.,-30.,12.));
#3467=CARTESIAN_POINT('Origin',(60.,-30.,-5.));
#3468=CARTESIAN_POINT('',(0.,0.,0.));
#3469=CARTESIAN_POINT('Origin',(60.,0.,10.));
#3470=CARTESIAN_POINT('',(55.,6.12323399573677E-16,20.));
#3471=CARTESIAN_POINT('Origin',(60.,0.,20.));
#3472=CARTESIAN_POINT('',(55.,6.12323399573677E-16,0.));
#3473=CARTESIAN_POINT('',(55.,6.12323399573677E-16,10.));
#3474=CARTESIAN_POINT('Origin',(60.,0.,0.));
#3475=CARTESIAN_POINT('Origin',(0.,0.,10.));
#3476=CARTESIAN_POINT('',(-5.,6.12323399573677E-16,20.));
#3477=CARTESIAN_POINT('Origin',(0.,0.,20.));
#3478=CARTESIAN_POINT('',(-5.,6.12323399573677E-16,0.));
#3479=CARTESIAN_POINT('',(-5.,6.12323399573677E-16,10.));
#3480=CARTESIAN_POINT('Origin',(0.,0.,0.));
#3481=CARTESIAN_POINT('Origin',(40.,60.,10.));
#3482=CARTESIAN_POINT('',(35.,60.,20.));
#3483=CARTESIAN_POINT('Origin',(40.,60.,20.));
#3484=CARTESIAN_POINT('',(35.,60.,0.));
#3485=CARTESIAN_POINT('',(35.,60.,10.));
#3486=CARTESIAN_POINT('Origin',(40.,60.,0.));
#3487=CARTESIAN_POINT('Origin',(-10.,-288.,0.));
#3488=CARTESIAN_POINT('',(-10.,-288.,0.));
#3489=CARTESIAN_POINT('',(-10.,-18.,0.));
#3490=CARTESIAN_POINT('',(-10.,-288.,0.));
#3491=CARTESIAN_POINT('',(-10.,-18.,20.));
#3492=CARTESIAN_POINT('',(-10.,-18.,0.));
#3493=CARTESIAN_POINT('',(-10.,-288.,20.));
#3494=CARTESIAN_POINT('',(-10.,-288.,20.));
#3495=CARTESIAN_POINT('',(-10.,-288.,0.));
#3496=CARTESIAN_POINT('Origin',(-30.,-288.,0.));
#3497=CARTESIAN_POINT('',(-35.,-288.,0.));
#3498=CARTESIAN_POINT('',(-30.,-288.,0.));
#3499=CARTESIAN_POINT('',(-35.,-288.,20.));
#3500=CARTESIAN_POINT('',(-30.,-288.,20.));
#3501=CARTESIAN_POINT('',(-35.,-288.,0.));
#3502=CARTESIAN_POINT('Origin',(-30.,-18.,0.));
#3503=CARTESIAN_POINT('',(95.,-18.,0.));
#3504=CARTESIAN_POINT('',(-30.,-18.,0.));
#3505=CARTESIAN_POINT('',(95.,-18.,20.));
#3506=CARTESIAN_POINT('',(95.,-18.,0.));
#3507=CARTESIAN_POINT('',(-30.,-18.,20.));
#3508=CARTESIAN_POINT('Origin',(90.,85.,0.));
#3509=CARTESIAN_POINT('',(95.,85.,0.));
#3510=CARTESIAN_POINT('',(-35.,85.,0.));
#3511=CARTESIAN_POINT('',(60.,85.,0.));
#3512=CARTESIAN_POINT('',(-35.,85.,20.));
#3513=CARTESIAN_POINT('',(-35.,85.,0.));
#3514=CARTESIAN_POINT('',(95.,85.,20.));
#3515=CARTESIAN_POINT('',(60.,85.,20.));
#3516=CARTESIAN_POINT('',(95.,85.,0.));
#3517=CARTESIAN_POINT('Origin',(95.,-18.,0.));
#3518=CARTESIAN_POINT('',(95.,6.5,0.));
#3519=CARTESIAN_POINT('',(95.,6.5,20.));
#3520=CARTESIAN_POINT('Origin',(-35.,80.,0.));
#3521=CARTESIAN_POINT('',(-35.,55.5,0.));
#3522=CARTESIAN_POINT('',(-35.,55.5,20.));
#3523=CARTESIAN_POINT('Origin',(30.,31.,20.));
#3524=CARTESIAN_POINT('Origin',(30.,31.,0.));
#3525=CARTESIAN_POINT('',(0.,0.,0.));
#3526=CARTESIAN_POINT('Origin',(0.,0.,4.));
#3527=CARTESIAN_POINT('',(-7.,8.57252759403147E-16,8.));
#3528=CARTESIAN_POINT('Origin',(0.,0.,8.));
#3529=CARTESIAN_POINT('',(-7.,8.57252759403147E-16,0.));
#3530=CARTESIAN_POINT('',(-7.,8.57252759403147E-16,4.));
#3531=CARTESIAN_POINT('Origin',(0.,0.,0.));
#3532=CARTESIAN_POINT('Origin',(20.,0.,4.));
#3533=CARTESIAN_POINT('',(13.,8.57252759403147E-16,8.));
#3534=CARTESIAN_POINT('Origin',(20.,0.,8.));
#3535=CARTESIAN_POINT('',(13.,8.57252759403147E-16,0.));
#3536=CARTESIAN_POINT('',(13.,8.57252759403147E-16,4.));
#3537=CARTESIAN_POINT('Origin',(20.,0.,0.));
#3538=CARTESIAN_POINT('Origin',(20.,12.,0.));
#3539=CARTESIAN_POINT('',(20.,12.,0.));
#3540=CARTESIAN_POINT('',(0.,12.,0.));
#3541=CARTESIAN_POINT('',(20.,12.,0.));
#3542=CARTESIAN_POINT('',(0.,12.,8.));
#3543=CARTESIAN_POINT('',(0.,12.,0.));
#3544=CARTESIAN_POINT('',(20.,12.,8.));
#3545=CARTESIAN_POINT('',(20.,12.,8.));
#3546=CARTESIAN_POINT('',(20.,12.,0.));
#3547=CARTESIAN_POINT('Origin',(20.,0.,0.));
#3548=CARTESIAN_POINT('',(20.,-12.,0.));
#3549=CARTESIAN_POINT('Origin',(20.,0.,0.));
#3550=CARTESIAN_POINT('',(20.,-12.,8.));
#3551=CARTESIAN_POINT('Origin',(20.,0.,8.));
#3552=CARTESIAN_POINT('',(20.,-12.,0.));
#3553=CARTESIAN_POINT('Origin',(0.,-12.,0.));
#3554=CARTESIAN_POINT('',(-1.46957615897682E-15,-12.,0.));
#3555=CARTESIAN_POINT('',(0.,-12.,0.));
#3556=CARTESIAN_POINT('',(-1.46957615897682E-15,-12.,8.));
#3557=CARTESIAN_POINT('',(0.,-12.,8.));
#3558=CARTESIAN_POINT('',(-1.46957615897682E-15,-12.,0.));
#3559=CARTESIAN_POINT('Origin',(0.,0.,0.));
#3560=CARTESIAN_POINT('Origin',(0.,0.,0.));
#3561=CARTESIAN_POINT('Origin',(0.,0.,8.));
#3562=CARTESIAN_POINT('Origin',(10.,0.,8.));
#3563=CARTESIAN_POINT('Origin',(10.,0.,0.));
#3564=CARTESIAN_POINT('',(0.,0.,0.));
#3565=CARTESIAN_POINT('Origin',(0.,0.,4.));
#3566=CARTESIAN_POINT('',(-7.,8.57252759403147E-16,8.));
#3567=CARTESIAN_POINT('Origin',(0.,0.,8.));
#3568=CARTESIAN_POINT('',(-7.,8.57252759403147E-16,0.));
#3569=CARTESIAN_POINT('',(-7.,8.57252759403147E-16,4.));
#3570=CARTESIAN_POINT('Origin',(0.,0.,0.));
#3571=CARTESIAN_POINT('Origin',(60.,0.,4.));
#3572=CARTESIAN_POINT('',(53.,8.57252759403147E-16,8.));
#3573=CARTESIAN_POINT('Origin',(60.,0.,8.));
#3574=CARTESIAN_POINT('',(53.,8.57252759403147E-16,0.));
#3575=CARTESIAN_POINT('',(53.,8.57252759403147E-16,4.));
#3576=CARTESIAN_POINT('Origin',(60.,0.,0.));
#3577=CARTESIAN_POINT('Origin',(60.,12.,0.));
#3578=CARTESIAN_POINT('',(60.,12.,0.));
#3579=CARTESIAN_POINT('',(0.,12.,0.));
#3580=CARTESIAN_POINT('',(60.,12.,0.));
#3581=CARTESIAN_POINT('',(0.,12.,8.));
#3582=CARTESIAN_POINT('',(0.,12.,0.));
#3583=CARTESIAN_POINT('',(60.,12.,8.));
#3584=CARTESIAN_POINT('',(60.,12.,8.));
#3585=CARTESIAN_POINT('',(60.,12.,0.));
#3586=CARTESIAN_POINT('Origin',(60.,0.,0.));
#3587=CARTESIAN_POINT('',(60.,-12.,0.));
#3588=CARTESIAN_POINT('Origin',(60.,0.,0.));
#3589=CARTESIAN_POINT('',(60.,-12.,8.));
#3590=CARTESIAN_POINT('Origin',(60.,0.,8.));
#3591=CARTESIAN_POINT('',(60.,-12.,0.));
#3592=CARTESIAN_POINT('Origin',(0.,-12.,0.));
#3593=CARTESIAN_POINT('',(-1.46957615897682E-15,-12.,0.));
#3594=CARTESIAN_POINT('',(0.,-12.,0.));
#3595=CARTESIAN_POINT('',(-1.46957615897682E-15,-12.,8.));
#3596=CARTESIAN_POINT('',(0.,-12.,8.));
#3597=CARTESIAN_POINT('',(-1.46957615897682E-15,-12.,0.));
#3598=CARTESIAN_POINT('Origin',(0.,0.,0.));
#3599=CARTESIAN_POINT('Origin',(0.,0.,0.));
#3600=CARTESIAN_POINT('Origin',(0.,0.,8.));
#3601=CARTESIAN_POINT('Origin',(30.,0.,8.));
#3602=CARTESIAN_POINT('Origin',(30.,0.,0.));
#3603=CARTESIAN_POINT('',(0.,0.,0.));
#3604=CARTESIAN_POINT('Origin',(80.,0.,4.));
#3605=CARTESIAN_POINT('',(73.,8.57252759403147E-16,8.));
#3606=CARTESIAN_POINT('Origin',(80.,0.,8.));
#3607=CARTESIAN_POINT('',(73.,8.57252759403147E-16,0.));
#3608=CARTESIAN_POINT('',(73.,8.57252759403147E-16,4.));
#3609=CARTESIAN_POINT('Origin',(80.,0.,0.));
#3610=CARTESIAN_POINT('Origin',(0.,0.,4.));
#3611=CARTESIAN_POINT('',(-7.,8.57252759403147E-16,8.));
#3612=CARTESIAN_POINT('Origin',(0.,0.,8.));
#3613=CARTESIAN_POINT('',(-7.,8.57252759403147E-16,0.));
#3614=CARTESIAN_POINT('',(-7.,8.57252759403147E-16,4.));
#3615=CARTESIAN_POINT('Origin',(0.,0.,0.));
#3616=CARTESIAN_POINT('Origin',(120.,0.,4.));
#3617=CARTESIAN_POINT('',(113.,8.57252759403147E-16,8.));
#3618=CARTESIAN_POINT('Origin',(120.,0.,8.));
#3619=CARTESIAN_POINT('',(113.,8.57252759403147E-16,0.));
#3620=CARTESIAN_POINT('',(113.,8.57252759403147E-16,4.));
#3621=CARTESIAN_POINT('Origin',(120.,0.,0.));
#3622=CARTESIAN_POINT('Origin',(120.,12.,0.));
#3623=CARTESIAN_POINT('',(120.,12.,0.));
#3624=CARTESIAN_POINT('',(0.,12.,0.));
#3625=CARTESIAN_POINT('',(120.,12.,0.));
#3626=CARTESIAN_POINT('',(0.,12.,8.));
#3627=CARTESIAN_POINT('',(0.,12.,0.));
#3628=CARTESIAN_POINT('',(120.,12.,8.));
#3629=CARTESIAN_POINT('',(120.,12.,8.));
#3630=CARTESIAN_POINT('',(120.,12.,0.));
#3631=CARTESIAN_POINT('Origin',(120.,-1.11022302462516E-15,0.));
#3632=CARTESIAN_POINT('',(120.,-12.,0.));
#3633=CARTESIAN_POINT('Origin',(120.,-1.11022302462516E-15,0.));
#3634=CARTESIAN_POINT('',(120.,-12.,8.));
#3635=CARTESIAN_POINT('Origin',(120.,-1.11022302462516E-15,8.));
#3636=CARTESIAN_POINT('',(120.,-12.,0.));
#3637=CARTESIAN_POINT('Origin',(0.,-12.,0.));
#3638=CARTESIAN_POINT('',(-1.46957615897682E-15,-12.,0.));
#3639=CARTESIAN_POINT('',(0.,-12.,0.));
#3640=CARTESIAN_POINT('',(-1.46957615897682E-15,-12.,8.));
#3641=CARTESIAN_POINT('',(0.,-12.,8.));
#3642=CARTESIAN_POINT('',(-1.46957615897682E-15,-12.,0.));
#3643=CARTESIAN_POINT('Origin',(0.,0.,0.));
#3644=CARTESIAN_POINT('Origin',(0.,0.,0.));
#3645=CARTESIAN_POINT('Origin',(0.,0.,8.));
#3646=CARTESIAN_POINT('Origin',(60.,0.,8.));
#3647=CARTESIAN_POINT('Origin',(60.,0.,0.));
#3648=CARTESIAN_POINT('',(0.,0.,0.));
#3649=CARTESIAN_POINT('Origin',(0.,0.,4.));
#3650=CARTESIAN_POINT('',(-7.,8.57252759403147E-16,8.));
#3651=CARTESIAN_POINT('Origin',(0.,0.,8.));
#3652=CARTESIAN_POINT('',(-7.,8.57252759403147E-16,0.));
#3653=CARTESIAN_POINT('',(-7.,8.57252759403147E-16,4.));
#3654=CARTESIAN_POINT('Origin',(0.,0.,0.));
#3655=CARTESIAN_POINT('Origin',(120.,0.,4.));
#3656=CARTESIAN_POINT('',(113.,8.57252759403147E-16,8.));
#3657=CARTESIAN_POINT('Origin',(120.,0.,8.));
#3658=CARTESIAN_POINT('',(113.,8.57252759403147E-16,0.));
#3659=CARTESIAN_POINT('',(113.,8.57252759403147E-16,4.));
#3660=CARTESIAN_POINT('Origin',(120.,0.,0.));
#3661=CARTESIAN_POINT('Origin',(120.,12.,0.));
#3662=CARTESIAN_POINT('',(120.,12.,0.));
#3663=CARTESIAN_POINT('',(0.,12.,0.));
#3664=CARTESIAN_POINT('',(120.,12.,0.));
#3665=CARTESIAN_POINT('',(0.,12.,8.));
#3666=CARTESIAN_POINT('',(0.,12.,0.));
#3667=CARTESIAN_POINT('',(120.,12.,8.));
#3668=CARTESIAN_POINT('',(120.,12.,8.));
#3669=CARTESIAN_POINT('',(120.,12.,0.));
#3670=CARTESIAN_POINT('Origin',(120.,-1.11022302462516E-15,0.));
#3671=CARTESIAN_POINT('',(120.,-12.,0.));
#3672=CARTESIAN_POINT('Origin',(120.,-1.11022302462516E-15,0.));
#3673=CARTESIAN_POINT('',(120.,-12.,8.));
#3674=CARTESIAN_POINT('Origin',(120.,-1.11022302462516E-15,8.));
#3675=CARTESIAN_POINT('',(120.,-12.,0.));
#3676=CARTESIAN_POINT('Origin',(0.,-12.,0.));
#3677=CARTESIAN_POINT('',(-1.46957615897682E-15,-12.,0.));
#3678=CARTESIAN_POINT('',(0.,-12.,0.));
#3679=CARTESIAN_POINT('',(-1.46957615897682E-15,-12.,8.));
#3680=CARTESIAN_POINT('',(0.,-12.,8.));
#3681=CARTESIAN_POINT('',(-1.46957615897682E-15,-12.,0.));
#3682=CARTESIAN_POINT('Origin',(0.,0.,0.));
#3683=CARTESIAN_POINT('Origin',(0.,0.,0.));
#3684=CARTESIAN_POINT('Origin',(0.,0.,8.));
#3685=CARTESIAN_POINT('Origin',(60.,0.,8.));
#3686=CARTESIAN_POINT('Origin',(60.,0.,0.));
#3687=CARTESIAN_POINT('',(0.,0.,0.));
#3688=CARTESIAN_POINT('Origin',(0.,0.,4.));
#3689=CARTESIAN_POINT('',(-7.,8.57252759403147E-16,8.));
#3690=CARTESIAN_POINT('Origin',(0.,0.,8.));
#3691=CARTESIAN_POINT('',(-7.,8.57252759403147E-16,0.));
#3692=CARTESIAN_POINT('',(-7.,8.57252759403147E-16,4.));
#3693=CARTESIAN_POINT('Origin',(0.,0.,0.));
#3694=CARTESIAN_POINT('Origin',(140.,0.,4.));
#3695=CARTESIAN_POINT('',(133.,8.57252759403147E-16,8.));
#3696=CARTESIAN_POINT('Origin',(140.,0.,8.));
#3697=CARTESIAN_POINT('',(133.,8.57252759403147E-16,0.));
#3698=CARTESIAN_POINT('',(133.,8.57252759403147E-16,4.));
#3699=CARTESIAN_POINT('Origin',(140.,0.,0.));
#3700=CARTESIAN_POINT('Origin',(260.,12.,0.));
#3701=CARTESIAN_POINT('',(260.,12.,0.));
#3702=CARTESIAN_POINT('',(0.,12.,0.));
#3703=CARTESIAN_POINT('',(260.,12.,0.));
#3704=CARTESIAN_POINT('',(0.,12.,8.));
#3705=CARTESIAN_POINT('',(0.,12.,0.));
#3706=CARTESIAN_POINT('',(260.,12.,8.));
#3707=CARTESIAN_POINT('',(260.,12.,8.));
#3708=CARTESIAN_POINT('',(260.,12.,0.));
#3709=CARTESIAN_POINT('Origin',(260.,-1.11022302462516E-15,0.));
#3710=CARTESIAN_POINT('',(260.,-12.,0.));
#3711=CARTESIAN_POINT('Origin',(260.,-1.11022302462516E-15,0.));
#3712=CARTESIAN_POINT('',(260.,-12.,8.));
#3713=CARTESIAN_POINT('Origin',(260.,-1.11022302462516E-15,8.));
#3714=CARTESIAN_POINT('',(260.,-12.,0.));
#3715=CARTESIAN_POINT('Origin',(0.,-12.,0.));
#3716=CARTESIAN_POINT('',(-1.46957615897682E-15,-12.,0.));
#3717=CARTESIAN_POINT('',(0.,-12.,0.));
#3718=CARTESIAN_POINT('',(-1.46957615897682E-15,-12.,8.));
#3719=CARTESIAN_POINT('',(0.,-12.,8.));
#3720=CARTESIAN_POINT('',(-1.46957615897682E-15,-12.,0.));
#3721=CARTESIAN_POINT('Origin',(0.,0.,0.));
#3722=CARTESIAN_POINT('Origin',(0.,0.,0.));
#3723=CARTESIAN_POINT('Origin',(0.,0.,8.));
#3724=CARTESIAN_POINT('Origin',(130.,0.,8.));
#3725=CARTESIAN_POINT('Origin',(130.,0.,0.));
#3726=CARTESIAN_POINT('',(0.,0.,0.));
#3727=CARTESIAN_POINT('Origin',(0.,0.,0.));
#3728=CARTESIAN_POINT('',(-15.,-1.83697019872103E-15,4.));
#3729=CARTESIAN_POINT('Origin',(0.,0.,4.));
#3730=CARTESIAN_POINT('',(-15.,-1.83697019872103E-15,0.));
#3731=CARTESIAN_POINT('',(-15.,-1.83697019872103E-15,0.));
#3732=CARTESIAN_POINT('Origin',(0.,0.,0.));
#3733=CARTESIAN_POINT('Origin',(0.,0.,4.));
#3734=CARTESIAN_POINT('Origin',(0.,0.,0.));
#3735=CARTESIAN_POINT('',(0.,0.,0.));
#3736=CARTESIAN_POINT('Origin',(0.,0.,0.));
#3737=CARTESIAN_POINT('',(-5.,-6.12323399573677E-16,8.));
#3738=CARTESIAN_POINT('Origin',(0.,0.,8.));
#3739=CARTESIAN_POINT('',(-5.,-6.12323399573677E-16,0.));
#3740=CARTESIAN_POINT('',(-5.,-6.12323399573677E-16,0.));
#3741=CARTESIAN_POINT('Origin',(0.,0.,0.));
#3742=CARTESIAN_POINT('Origin',(0.,0.,0.));
#3743=CARTESIAN_POINT('',(-7.,-8.57252759403147E-16,8.));
#3744=CARTESIAN_POINT('Origin',(0.,0.,8.));
#3745=CARTESIAN_POINT('',(-7.,-8.57252759403147E-16,0.));
#3746=CARTESIAN_POINT('',(-7.,-8.57252759403147E-16,0.));
#3747=CARTESIAN_POINT('Origin',(0.,0.,0.));
#3748=CARTESIAN_POINT('Origin',(0.,0.,8.));
#3749=CARTESIAN_POINT('Origin',(0.,0.,0.));
#3750=CARTESIAN_POINT('',(0.,0.,0.));
#3751=CARTESIAN_POINT('Origin',(0.,0.,38.5));
#3752=CARTESIAN_POINT('',(-4.,-4.89858719658941E-16,38.));
#3753=CARTESIAN_POINT('Origin',(0.,0.,38.));
#3754=CARTESIAN_POINT('',(-4.,-4.89858719658941E-16,39.));
#3755=CARTESIAN_POINT('',(-4.,-4.89858719658941E-16,38.5));
#3756=CARTESIAN_POINT('Origin',(0.,0.,39.));
#3757=CARTESIAN_POINT('Origin',(8.,0.,38.));
#3758=CARTESIAN_POINT('',(-5.,6.12323399573677E-16,38.));
#3759=CARTESIAN_POINT('Origin',(0.,0.,38.));
#3760=CARTESIAN_POINT('Origin',(4.,0.,39.));
#3761=CARTESIAN_POINT('',(-5.,-6.12323399573677E-16,39.));
#3762=CARTESIAN_POINT('Origin',(0.,0.,39.));
#3763=CARTESIAN_POINT('Origin',(0.,0.,0.));
#3764=CARTESIAN_POINT('',(-5.,-6.12323399573677E-16,40.));
#3765=CARTESIAN_POINT('Origin',(0.,0.,40.));
#3766=CARTESIAN_POINT('',(-5.,-6.12323399573677E-16,0.));
#3767=CARTESIAN_POINT('Origin',(0.,0.,0.));
#3768=CARTESIAN_POINT('',(-8.,-9.79717439317883E-16,0.));
#3769=CARTESIAN_POINT('Origin',(0.,0.,0.));
#3770=CARTESIAN_POINT('',(-5.,-6.12323399573677E-16,0.));
#3771=CARTESIAN_POINT('Origin',(0.,0.,0.));
#3772=CARTESIAN_POINT('Origin',(0.,0.,-4.));
#3773=CARTESIAN_POINT('',(-8.,-9.79717439317883E-16,-4.));
#3774=CARTESIAN_POINT('',(-8.,-9.79717439317883E-16,-4.));
#3775=CARTESIAN_POINT('Origin',(0.,0.,-4.));
#3776=CARTESIAN_POINT('Origin',(0.,0.,-4.));
#3777=CARTESIAN_POINT('Origin',(0.,0.,0.));
#3778=CARTESIAN_POINT('',(-5.,-6.12323399573677E-16,0.));
#3779=CARTESIAN_POINT('Origin',(0.,0.,40.));
#3780=CARTESIAN_POINT('',(0.,0.,0.));
#3781=CARTESIAN_POINT('Origin',(0.,0.,0.5));
#3782=CARTESIAN_POINT('',(-10.,1.22464679914735E-15,1.));
#3783=CARTESIAN_POINT('Origin',(0.,0.,1.));
#3784=CARTESIAN_POINT('',(-9.,-1.10218211923262E-15,0.));
#3785=CARTESIAN_POINT('',(-9.5,-1.16341445918999E-15,0.5));
#3786=CARTESIAN_POINT('Origin',(0.,0.,0.));
#3787=CARTESIAN_POINT('Origin',(0.,0.,0.));
#3788=CARTESIAN_POINT('',(-10.,-1.22464679914735E-15,7.));
#3789=CARTESIAN_POINT('Origin',(0.,0.,7.));
#3790=CARTESIAN_POINT('',(-10.,-1.22464679914735E-15,0.));
#3791=CARTESIAN_POINT('Origin',(0.,0.,0.));
#3792=CARTESIAN_POINT('',(-6.,7.34788079488412E-16,0.));
#3793=CARTESIAN_POINT('Origin',(0.,0.,0.));
#3794=CARTESIAN_POINT('Origin',(0.,0.,7.5));
#3795=CARTESIAN_POINT('',(-9.,1.10218211923262E-15,8.));
#3796=CARTESIAN_POINT('Origin',(0.,0.,8.));
#3797=CARTESIAN_POINT('',(-9.5,-1.16341445918999E-15,7.5));
#3798=CARTESIAN_POINT('Origin',(0.,0.,8.));
#3799=CARTESIAN_POINT('',(-6.,-7.34788079488412E-16,8.));
#3800=CARTESIAN_POINT('Origin',(0.,0.,8.));
#3801=CARTESIAN_POINT('Origin',(0.,0.,0.5));
#3802=CARTESIAN_POINT('',(-5.,-6.12323399573677E-16,1.));
#3803=CARTESIAN_POINT('Origin',(0.,0.,1.));
#3804=CARTESIAN_POINT('',(-5.5,-6.73555739531044E-16,0.5));
#3805=CARTESIAN_POINT('Origin',(0.,0.,0.));
#3806=CARTESIAN_POINT('',(-5.,6.12323399573677E-16,7.));
#3807=CARTESIAN_POINT('Origin',(0.,0.,7.));
#3808=CARTESIAN_POINT('',(-5.,-6.12323399573677E-16,0.));
#3809=CARTESIAN_POINT('Origin',(0.,0.,7.5));
#3810=CARTESIAN_POINT('',(-5.5,-6.73555739531044E-16,7.5));
#3811=CARTESIAN_POINT('',(0.,0.,0.));
#3812=CARTESIAN_POINT('Origin',(0.,0.,0.));
#3813=CARTESIAN_POINT('',(-5.,-6.12323399573677E-16,2.));
#3814=CARTESIAN_POINT('Origin',(0.,0.,2.));
#3815=CARTESIAN_POINT('',(-5.,-6.12323399573677E-16,0.));
#3816=CARTESIAN_POINT('',(-5.,-6.12323399573677E-16,0.));
#3817=CARTESIAN_POINT('Origin',(0.,0.,0.));
#3818=CARTESIAN_POINT('Origin',(0.,0.,0.));
#3819=CARTESIAN_POINT('',(-10.,-1.22464679914735E-15,2.));
#3820=CARTESIAN_POINT('Origin',(0.,0.,2.));
#3821=CARTESIAN_POINT('',(-10.,-1.22464679914735E-15,0.));
#3822=CARTESIAN_POINT('',(-10.,-1.22464679914735E-15,0.));
#3823=CARTESIAN_POINT('Origin',(0.,0.,0.));
#3824=CARTESIAN_POINT('Origin',(0.,0.,2.));
#3825=CARTESIAN_POINT('Origin',(0.,0.,0.));
#3826=CARTESIAN_POINT('',(0.,0.,0.));
#3827=CARTESIAN_POINT('Origin',(0.,0.,95.5));
#3828=CARTESIAN_POINT('',(-4.,-4.89858719658941E-16,95.));
#3829=CARTESIAN_POINT('Origin',(0.,0.,95.));
#3830=CARTESIAN_POINT('',(-4.,-4.89858719658941E-16,96.));
#3831=CARTESIAN_POINT('',(-4.,-4.89858719658941E-16,95.5));
#3832=CARTESIAN_POINT('Origin',(0.,0.,96.));
#3833=CARTESIAN_POINT('Origin',(8.,0.,95.));
#3834=CARTESIAN_POINT('',(-5.,6.12323399573677E-16,95.));
#3835=CARTESIAN_POINT('Origin',(0.,0.,95.));
#3836=CARTESIAN_POINT('Origin',(4.,0.,96.));
#3837=CARTESIAN_POINT('',(-5.,-6.12323399573677E-16,96.));
#3838=CARTESIAN_POINT('Origin',(0.,0.,96.));
#3839=CARTESIAN_POINT('Origin',(0.,0.,0.));
#3840=CARTESIAN_POINT('',(-5.,-6.12323399573677E-16,97.));
#3841=CARTESIAN_POINT('Origin',(0.,0.,97.));
#3842=CARTESIAN_POINT('',(-5.,-6.12323399573677E-16,0.));
#3843=CARTESIAN_POINT('Origin',(0.,0.,0.));
#3844=CARTESIAN_POINT('',(-8.,-9.79717439317883E-16,0.));
#3845=CARTESIAN_POINT('Origin',(0.,0.,0.));
#3846=CARTESIAN_POINT('',(-5.,-6.12323399573677E-16,0.));
#3847=CARTESIAN_POINT('Origin',(0.,0.,0.));
#3848=CARTESIAN_POINT('Origin',(0.,0.,-2.));
#3849=CARTESIAN_POINT('',(-8.,-9.79717439317883E-16,-2.));
#3850=CARTESIAN_POINT('',(-8.,-9.79717439317883E-16,-2.));
#3851=CARTESIAN_POINT('Origin',(0.,0.,-2.));
#3852=CARTESIAN_POINT('Origin',(0.,0.,-2.));
#3853=CARTESIAN_POINT('Origin',(0.,0.,0.));
#3854=CARTESIAN_POINT('',(-5.,-6.12323399573677E-16,0.));
#3855=CARTESIAN_POINT('Origin',(0.,0.,97.));
#3856=CARTESIAN_POINT('',(0.,0.,0.));
#3857=CARTESIAN_POINT('Origin',(0.,0.,0.));
#3858=CARTESIAN_POINT('',(-5.,-6.12323399573677E-16,76.));
#3859=CARTESIAN_POINT('Origin',(0.,0.,76.));
#3860=CARTESIAN_POINT('',(-5.,-6.12323399573677E-16,0.));
#3861=CARTESIAN_POINT('',(-5.,-6.12323399573677E-16,0.));
#3862=CARTESIAN_POINT('Origin',(0.,0.,0.));
#3863=CARTESIAN_POINT('Origin',(0.,0.,0.));
#3864=CARTESIAN_POINT('',(-10.,-1.22464679914735E-15,76.));
#3865=CARTESIAN_POINT('Origin',(0.,0.,76.));
#3866=CARTESIAN_POINT('',(-10.,-1.22464679914735E-15,0.));
#3867=CARTESIAN_POINT('',(-10.,-1.22464679914735E-15,0.));
#3868=CARTESIAN_POINT('Origin',(0.,0.,0.));
#3869=CARTESIAN_POINT('Origin',(0.,0.,76.));
#3870=CARTESIAN_POINT('Origin',(0.,0.,0.));
#3871=CARTESIAN_POINT('',(0.,0.,0.));
#3872=CARTESIAN_POINT('Origin',(-1.,0.,1.));
#3873=CARTESIAN_POINT('',(-1.,3.87298334620742,0.));
#3874=CARTESIAN_POINT('',(-1.,3.87298334620742,1.));
#3875=CARTESIAN_POINT('',(-1.,3.87298334620742,0.));
#3876=CARTESIAN_POINT('',(-1.,7.93725393319377,0.));
#3877=CARTESIAN_POINT('',(-1.,0.,0.));
#3878=CARTESIAN_POINT('',(-1.,7.93725393319377,1.));
#3879=CARTESIAN_POINT('',(-1.,7.93725393319377,0.));
#3880=CARTESIAN_POINT('',(-1.,0.,1.));
#3881=CARTESIAN_POINT('Origin',(1.,16.,1.));
#3882=CARTESIAN_POINT('',(1.,3.87298334620742,1.));
#3883=CARTESIAN_POINT('',(1.,3.87298334620742,0.));
#3884=CARTESIAN_POINT('',(1.,3.87298334620742,0.));
#3885=CARTESIAN_POINT('',(1.,7.93725393319377,1.));
#3886=CARTESIAN_POINT('',(1.,8.,1.));
#3887=CARTESIAN_POINT('',(1.,7.93725393319377,0.));
#3888=CARTESIAN_POINT('',(1.,7.93725393319377,0.));
#3889=CARTESIAN_POINT('',(1.,8.,0.));
#3890=CARTESIAN_POINT('Origin',(0.,0.,0.));
#3891=CARTESIAN_POINT('Origin',(0.,0.,0.));
#3892=CARTESIAN_POINT('Origin',(0.,0.,0.));
#3893=CARTESIAN_POINT('Origin',(0.,0.,0.));
#3894=CARTESIAN_POINT('Origin',(0.,0.,1.));
#3895=CARTESIAN_POINT('Origin',(0.,0.,0.));
#3896=CARTESIAN_POINT('Origin',(0.,0.,1.));
#3897=CARTESIAN_POINT('Origin',(0.,0.,1.));
#3898=CARTESIAN_POINT('',(0.,0.,0.));
#3899=CARTESIAN_POINT('Origin',(0.,0.,31.5));
#3900=CARTESIAN_POINT('',(-4.,-4.89858719658941E-16,31.));
#3901=CARTESIAN_POINT('Origin',(0.,0.,31.));
#3902=CARTESIAN_POINT('',(-4.,-4.89858719658941E-16,32.));
#3903=CARTESIAN_POINT('',(-4.,-4.89858719658941E-16,31.5));
#3904=CARTESIAN_POINT('Origin',(0.,0.,32.));
#3905=CARTESIAN_POINT('Origin',(8.,0.,31.));
#3906=CARTESIAN_POINT('',(-5.,6.12323399573677E-16,31.));
#3907=CARTESIAN_POINT('Origin',(0.,0.,31.));
#3908=CARTESIAN_POINT('Origin',(4.,0.,32.));
#3909=CARTESIAN_POINT('',(-5.,-6.12323399573677E-16,32.));
#3910=CARTESIAN_POINT('Origin',(0.,0.,32.));
#3911=CARTESIAN_POINT('Origin',(0.,0.,0.));
#3912=CARTESIAN_POINT('',(-5.,-6.12323399573677E-16,33.));
#3913=CARTESIAN_POINT('Origin',(0.,0.,33.));
#3914=CARTESIAN_POINT('',(-5.,-6.12323399573677E-16,0.));
#3915=CARTESIAN_POINT('Origin',(0.,0.,0.));
#3916=CARTESIAN_POINT('',(-8.,-9.79717439317883E-16,0.));
#3917=CARTESIAN_POINT('Origin',(0.,0.,0.));
#3918=CARTESIAN_POINT('',(-5.,-6.12323399573677E-16,0.));
#3919=CARTESIAN_POINT('Origin',(0.,0.,0.));
#3920=CARTESIAN_POINT('Origin',(0.,0.,-2.));
#3921=CARTESIAN_POINT('',(-8.,-9.79717439317883E-16,-2.));
#3922=CARTESIAN_POINT('',(-8.,-9.79717439317883E-16,-2.));
#3923=CARTESIAN_POINT('Origin',(0.,0.,-2.));
#3924=CARTESIAN_POINT('Origin',(0.,0.,-2.));
#3925=CARTESIAN_POINT('Origin',(0.,0.,0.));
#3926=CARTESIAN_POINT('',(-5.,-6.12323399573677E-16,0.));
#3927=CARTESIAN_POINT('Origin',(0.,0.,33.));
#3928=CARTESIAN_POINT('',(0.,0.,0.));
#3929=CARTESIAN_POINT('Origin',(0.,0.,0.));
#3930=CARTESIAN_POINT('',(-5.,-6.12323399573677E-16,1.));
#3931=CARTESIAN_POINT('Origin',(0.,0.,1.));
#3932=CARTESIAN_POINT('',(-5.,-6.12323399573677E-16,0.));
#3933=CARTESIAN_POINT('',(-5.,-6.12323399573677E-16,0.));
#3934=CARTESIAN_POINT('Origin',(0.,0.,0.));
#3935=CARTESIAN_POINT('Origin',(0.,0.,0.));
#3936=CARTESIAN_POINT('',(-10.,-1.22464679914735E-15,1.));
#3937=CARTESIAN_POINT('Origin',(0.,0.,1.));
#3938=CARTESIAN_POINT('',(-10.,-1.22464679914735E-15,0.));
#3939=CARTESIAN_POINT('',(-10.,-1.22464679914735E-15,0.));
#3940=CARTESIAN_POINT('Origin',(0.,0.,0.));
#3941=CARTESIAN_POINT('Origin',(0.,0.,1.));
#3942=CARTESIAN_POINT('Origin',(0.,0.,0.));
#3943=CARTESIAN_POINT('',(0.,0.,0.));
#3944=CARTESIAN_POINT('Origin',(0.,0.,0.));
#3945=CARTESIAN_POINT('',(-5.,-6.12323399573677E-16,12.));
#3946=CARTESIAN_POINT('Origin',(0.,0.,12.));
#3947=CARTESIAN_POINT('',(-5.,-6.12323399573677E-16,0.));
#3948=CARTESIAN_POINT('',(-5.,-6.12323399573677E-16,0.));
#3949=CARTESIAN_POINT('Origin',(0.,0.,0.));
#3950=CARTESIAN_POINT('Origin',(0.,0.,0.));
#3951=CARTESIAN_POINT('',(-10.,-1.22464679914735E-15,12.));
#3952=CARTESIAN_POINT('Origin',(0.,0.,12.));
#3953=CARTESIAN_POINT('',(-10.,-1.22464679914735E-15,0.));
#3954=CARTESIAN_POINT('',(-10.,-1.22464679914735E-15,0.));
#3955=CARTESIAN_POINT('Origin',(0.,0.,0.));
#3956=CARTESIAN_POINT('Origin',(0.,0.,12.));
#3957=CARTESIAN_POINT('Origin',(0.,0.,0.));
#3958=CARTESIAN_POINT('',(0.,0.,0.));
#3959=CARTESIAN_POINT('',(0.,0.,300.));
#3960=CARTESIAN_POINT('',(8.88178419700125E-15,-28.,300.));
#3961=CARTESIAN_POINT('',(60.,-28.,300.));
#3962=CARTESIAN_POINT('',(7.77557373722978,-48.,318.426623484972));
#3963=CARTESIAN_POINT('',(40.,16.,360.));
#3964=CARTESIAN_POINT('',(112.624845060065,-68.,376.792969122429));
#3965=CARTESIAN_POINT('',(32.2717557721802,-76.,129.521092351342));
#3966=CARTESIAN_POINT('',(8.88178419700125E-15,-28.,300.));
#3967=CARTESIAN_POINT('',(0.,0.,300.));
#3968=CARTESIAN_POINT('',(0.,-20.,300.));
#3969=CARTESIAN_POINT('',(7.77557373722989,-28.,318.426623484972));
#3970=CARTESIAN_POINT('',(60.,-28.,300.));
#3971=CARTESIAN_POINT('',(77.6750879524531,-28.,357.33752057661));
#3972=CARTESIAN_POINT('',(7.77557373722976,-48.,318.426623484972));
#3973=CARTESIAN_POINT('',(77.6750879524528,-48.,357.33752057661));
#3974=CARTESIAN_POINT('',(112.624845060064,-48.,376.792969122429));
#3975=CARTESIAN_POINT('',(39.9999999999999,16.,360.));
#3976=CARTESIAN_POINT('',(69.3577969819729,16.,243.646573937997));
#3977=CARTESIAN_POINT('',(112.624845060065,-68.,376.792969122429));
#3978=CARTESIAN_POINT('',(69.357796981973,-68.,243.646573937998));
#3979=CARTESIAN_POINT('',(60.,0.,300.));
#3980=CARTESIAN_POINT('',(40.,-20.,360.));
#3981=CARTESIAN_POINT('',(0.,-36.,300.));
#3982=CARTESIAN_POINT('',(60.,-20.,300.));
#3983=CARTESIAN_POINT('',(40.,0.,360.));
#3984=CARTESIAN_POINT('',(0.,-38.,300.));
#3985=CARTESIAN_POINT('',(60.,-36.,300.));
#3986=CARTESIAN_POINT('',(40.,16.,360.));
#3987=CARTESIAN_POINT('',(7.7755737372299,-56.,318.426623484972));
#3988=CARTESIAN_POINT('',(77.675087952453,-56.,357.33752057661));
#3989=CARTESIAN_POINT('',(112.624845060065,-76.,376.792969122429));
#3990=CARTESIAN_POINT('',(69.357796981973,-76.,243.646573937997));
#3991=CARTESIAN_POINT('',(7.77557373722989,-27.,318.426623484972));
#3992=CARTESIAN_POINT('',(69.3577969819729,17.,243.646573937997));
#3993=CARTESIAN_POINT('',(7.77557373722991,-27.,318.426623484972));
#3994=CARTESIAN_POINT('',(7.77557373722989,-36.,318.426623484972));
#3995=CARTESIAN_POINT('',(69.3577969819729,8.,243.646573937997));
#3996=CARTESIAN_POINT('',(60.,-38.,300.));
#3997=CARTESIAN_POINT('',(40.,18.,360.));
#3998=CARTESIAN_POINT('',(7.7755737372299,-58.,318.426623484972));
#3999=CARTESIAN_POINT('',(77.675087952453,-58.,357.33752057661));
#4000=CARTESIAN_POINT('',(112.624845060065,-78.,376.792969122429));
#4001=CARTESIAN_POINT('',(69.3577969819729,-78.,243.646573937997));
#4002=CARTESIAN_POINT('',(77.6750879524531,-27.,357.33752057661));
#4003=CARTESIAN_POINT('',(112.624845060064,-47.,376.792969122429));
#4004=CARTESIAN_POINT('',(77.675087952453,-27.,357.33752057661));
#4005=CARTESIAN_POINT('',(112.624845060065,-47.,376.792969122429));
#4006=CARTESIAN_POINT('',(69.3577969819729,17.,243.646573937997));
#4007=CARTESIAN_POINT('',(77.675087952453,-36.,357.33752057661));
#4008=CARTESIAN_POINT('',(112.624845060065,-56.,376.792969122429));
#4009=UNCERTAINTY_MEASURE_WITH_UNIT(LENGTH_MEASURE(0.01),#4049,
'DISTANCE_ACCURACY_VALUE',
'Maximum model space distance between geometric entities at asserted c
onnectivities');
#4010=UNCERTAINTY_MEASURE_WITH_UNIT(LENGTH_MEASURE(0.01),#4049,
'DISTANCE_ACCURACY_VALUE',
'Maximum model space distance between geometric entities at asserted c
onnectivities');
#4011=UNCERTAINTY_MEASURE_WITH_UNIT(LENGTH_MEASURE(0.01),#4049,
'DISTANCE_ACCURACY_VALUE',
'Maximum model space distance between geometric entities at asserted c
onnectivities');
#4012=UNCERTAINTY_MEASURE_WITH_UNIT(LENGTH_MEASURE(0.01),#4049,
'DISTANCE_ACCURACY_VALUE',
'Maximum model space distance between geometric entities at asserted c
onnectivities');
#4013=UNCERTAINTY_MEASURE_WITH_UNIT(LENGTH_MEASURE(0.01),#4049,
'DISTANCE_ACCURACY_VALUE',
'Maximum model space distance between geometric entities at asserted c
onnectivities');
#4014=UNCERTAINTY_MEASURE_WITH_UNIT(LENGTH_MEASURE(0.01),#4049,
'DISTANCE_ACCURACY_VALUE',
'Maximum model space distance between geometric entities at asserted c
onnectivities');
#4015=UNCERTAINTY_MEASURE_WITH_UNIT(LENGTH_MEASURE(0.01),#4049,
'DISTANCE_ACCURACY_VALUE',
'Maximum model space distance between geometric entities at asserted c
onnectivities');
#4016=UNCERTAINTY_MEASURE_WITH_UNIT(LENGTH_MEASURE(0.01),#4049,
'DISTANCE_ACCURACY_VALUE',
'Maximum model space distance between geometric entities at asserted c
onnectivities');
#4017=UNCERTAINTY_MEASURE_WITH_UNIT(LENGTH_MEASURE(0.01),#4049,
'DISTANCE_ACCURACY_VALUE',
'Maximum model space distance between geometric entities at asserted c
onnectivities');
#4018=UNCERTAINTY_MEASURE_WITH_UNIT(LENGTH_MEASURE(0.01),#4049,
'DISTANCE_ACCURACY_VALUE',
'Maximum model space distance between geometric entities at asserted c
onnectivities');
#4019=UNCERTAINTY_MEASURE_WITH_UNIT(LENGTH_MEASURE(0.01),#4049,
'DISTANCE_ACCURACY_VALUE',
'Maximum model space distance between geometric entities at asserted c
onnectivities');
#4020=UNCERTAINTY_MEASURE_WITH_UNIT(LENGTH_MEASURE(0.01),#4049,
'DISTANCE_ACCURACY_VALUE',
'Maximum model space distance between geometric entities at asserted c
onnectivities');
#4021=UNCERTAINTY_MEASURE_WITH_UNIT(LENGTH_MEASURE(0.01),#4049,
'DISTANCE_ACCURACY_VALUE',
'Maximum model space distance between geometric entities at asserted c
onnectivities');
#4022=UNCERTAINTY_MEASURE_WITH_UNIT(LENGTH_MEASURE(0.01),#4049,
'DISTANCE_ACCURACY_VALUE',
'Maximum model space distance between geometric entities at asserted c
onnectivities');
#4023=UNCERTAINTY_MEASURE_WITH_UNIT(LENGTH_MEASURE(0.01),#4049,
'DISTANCE_ACCURACY_VALUE',
'Maximum model space distance between geometric entities at asserted c
onnectivities');
#4024=UNCERTAINTY_MEASURE_WITH_UNIT(LENGTH_MEASURE(0.01),#4049,
'DISTANCE_ACCURACY_VALUE',
'Maximum model space distance between geometric entities at asserted c
onnectivities');
#4025=UNCERTAINTY_MEASURE_WITH_UNIT(LENGTH_MEASURE(0.01),#4049,
'DISTANCE_ACCURACY_VALUE',
'Maximum model space distance between geometric entities at asserted c
onnectivities');
#4026=UNCERTAINTY_MEASURE_WITH_UNIT(LENGTH_MEASURE(0.01),#4049,
'DISTANCE_ACCURACY_VALUE',
'Maximum model space distance between geometric entities at asserted c
onnectivities');
#4027=UNCERTAINTY_MEASURE_WITH_UNIT(LENGTH_MEASURE(0.01),#4049,
'DISTANCE_ACCURACY_VALUE',
'Maximum model space distance between geometric entities at asserted c
onnectivities');
#4028=UNCERTAINTY_MEASURE_WITH_UNIT(LENGTH_MEASURE(0.01),#4049,
'DISTANCE_ACCURACY_VALUE',
'Maximum model space distance between geometric entities at asserted c
onnectivities');
#4029=(
GEOMETRIC_REPRESENTATION_CONTEXT(3)
GLOBAL_UNCERTAINTY_ASSIGNED_CONTEXT((#4009))
GLOBAL_UNIT_ASSIGNED_CONTEXT((#4049,#4051,#4052))
REPRESENTATION_CONTEXT('','3D')
);
#4030=(
GEOMETRIC_REPRESENTATION_CONTEXT(3)
GLOBAL_UNCERTAINTY_ASSIGNED_CONTEXT((#4010))
GLOBAL_UNIT_ASSIGNED_CONTEXT((#4049,#4051,#4052))
REPRESENTATION_CONTEXT('','3D')
);
#4031=(
GEOMETRIC_REPRESENTATION_CONTEXT(3)
GLOBAL_UNCERTAINTY_ASSIGNED_CONTEXT((#4011))
GLOBAL_UNIT_ASSIGNED_CONTEXT((#4049,#4051,#4052))
REPRESENTATION_CONTEXT('','3D')
);
#4032=(
GEOMETRIC_REPRESENTATION_CONTEXT(3)
GLOBAL_UNCERTAINTY_ASSIGNED_CONTEXT((#4012))
GLOBAL_UNIT_ASSIGNED_CONTEXT((#4049,#4051,#4052))
REPRESENTATION_CONTEXT('','3D')
);
#4033=(
GEOMETRIC_REPRESENTATION_CONTEXT(3)
GLOBAL_UNCERTAINTY_ASSIGNED_CONTEXT((#4013))
GLOBAL_UNIT_ASSIGNED_CONTEXT((#4049,#4051,#4052))
REPRESENTATION_CONTEXT('','3D')
);
#4034=(
GEOMETRIC_REPRESENTATION_CONTEXT(3)
GLOBAL_UNCERTAINTY_ASSIGNED_CONTEXT((#4014))
GLOBAL_UNIT_ASSIGNED_CONTEXT((#4049,#4051,#4052))
REPRESENTATION_CONTEXT('','3D')
);
#4035=(
GEOMETRIC_REPRESENTATION_CONTEXT(3)
GLOBAL_UNCERTAINTY_ASSIGNED_CONTEXT((#4015))
GLOBAL_UNIT_ASSIGNED_CONTEXT((#4049,#4051,#4052))
REPRESENTATION_CONTEXT('','3D')
);
#4036=(
GEOMETRIC_REPRESENTATION_CONTEXT(3)
GLOBAL_UNCERTAINTY_ASSIGNED_CONTEXT((#4016))
GLOBAL_UNIT_ASSIGNED_CONTEXT((#4049,#4051,#4052))
REPRESENTATION_CONTEXT('','3D')
);
#4037=(
GEOMETRIC_REPRESENTATION_CONTEXT(3)
GLOBAL_UNCERTAINTY_ASSIGNED_CONTEXT((#4017))
GLOBAL_UNIT_ASSIGNED_CONTEXT((#4049,#4051,#4052))
REPRESENTATION_CONTEXT('','3D')
);
#4038=(
GEOMETRIC_REPRESENTATION_CONTEXT(3)
GLOBAL_UNCERTAINTY_ASSIGNED_CONTEXT((#4018))
GLOBAL_UNIT_ASSIGNED_CONTEXT((#4049,#4051,#4052))
REPRESENTATION_CONTEXT('','3D')
);
#4039=(
GEOMETRIC_REPRESENTATION_CONTEXT(3)
GLOBAL_UNCERTAINTY_ASSIGNED_CONTEXT((#4019))
GLOBAL_UNIT_ASSIGNED_CONTEXT((#4049,#4051,#4052))
REPRESENTATION_CONTEXT('','3D')
);
#4040=(
GEOMETRIC_REPRESENTATION_CONTEXT(3)
GLOBAL_UNCERTAINTY_ASSIGNED_CONTEXT((#4020))
GLOBAL_UNIT_ASSIGNED_CONTEXT((#4049,#4051,#4052))
REPRESENTATION_CONTEXT('','3D')
);
#4041=(
GEOMETRIC_REPRESENTATION_CONTEXT(3)
GLOBAL_UNCERTAINTY_ASSIGNED_CONTEXT((#4021))
GLOBAL_UNIT_ASSIGNED_CONTEXT((#4049,#4051,#4052))
REPRESENTATION_CONTEXT('','3D')
);
#4042=(
GEOMETRIC_REPRESENTATION_CONTEXT(3)
GLOBAL_UNCERTAINTY_ASSIGNED_CONTEXT((#4022))
GLOBAL_UNIT_ASSIGNED_CONTEXT((#4049,#4051,#4052))
REPRESENTATION_CONTEXT('','3D')
);
#4043=(
GEOMETRIC_REPRESENTATION_CONTEXT(3)
GLOBAL_UNCERTAINTY_ASSIGNED_CONTEXT((#4023))
GLOBAL_UNIT_ASSIGNED_CONTEXT((#4049,#4051,#4052))
REPRESENTATION_CONTEXT('','3D')
);
#4044=(
GEOMETRIC_REPRESENTATION_CONTEXT(3)
GLOBAL_UNCERTAINTY_ASSIGNED_CONTEXT((#4024))
GLOBAL_UNIT_ASSIGNED_CONTEXT((#4049,#4051,#4052))
REPRESENTATION_CONTEXT('','3D')
);
#4045=(
GEOMETRIC_REPRESENTATION_CONTEXT(3)
GLOBAL_UNCERTAINTY_ASSIGNED_CONTEXT((#4025))
GLOBAL_UNIT_ASSIGNED_CONTEXT((#4049,#4051,#4052))
REPRESENTATION_CONTEXT('','3D')
);
#4046=(
GEOMETRIC_REPRESENTATION_CONTEXT(3)
GLOBAL_UNCERTAINTY_ASSIGNED_CONTEXT((#4026))
GLOBAL_UNIT_ASSIGNED_CONTEXT((#4049,#4051,#4052))
REPRESENTATION_CONTEXT('','3D')
);
#4047=(
GEOMETRIC_REPRESENTATION_CONTEXT(3)
GLOBAL_UNCERTAINTY_ASSIGNED_CONTEXT((#4027))
GLOBAL_UNIT_ASSIGNED_CONTEXT((#4049,#4051,#4052))
REPRESENTATION_CONTEXT('','3D')
);
#4048=(
GEOMETRIC_REPRESENTATION_CONTEXT(3)
GLOBAL_UNCERTAINTY_ASSIGNED_CONTEXT((#4028))
GLOBAL_UNIT_ASSIGNED_CONTEXT((#4049,#4051,#4052))
REPRESENTATION_CONTEXT('','3D')
);
#4049=(
LENGTH_UNIT()
NAMED_UNIT(*)
SI_UNIT(.MILLI.,.METRE.)
);
#4050=(
LENGTH_UNIT()
NAMED_UNIT(*)
SI_UNIT($,.METRE.)
);
#4051=(
NAMED_UNIT(*)
PLANE_ANGLE_UNIT()
SI_UNIT($,.RADIAN.)
);
#4052=(
NAMED_UNIT(*)
SI_UNIT($,.STERADIAN.)
SOLID_ANGLE_UNIT()
);
#4053=SHAPE_DEFINITION_REPRESENTATION(#4072,#4142);
#4054=SHAPE_DEFINITION_REPRESENTATION(#4073,#4143);
#4055=SHAPE_DEFINITION_REPRESENTATION(#4074,#4144);
#4056=SHAPE_DEFINITION_REPRESENTATION(#4075,#4145);
#4057=SHAPE_DEFINITION_REPRESENTATION(#4076,#4146);
#4058=SHAPE_DEFINITION_REPRESENTATION(#4077,#4147);
#4059=SHAPE_DEFINITION_REPRESENTATION(#4078,#4148);
#4060=SHAPE_DEFINITION_REPRESENTATION(#4079,#4149);
#4061=SHAPE_DEFINITION_REPRESENTATION(#4080,#4150);
#4062=SHAPE_DEFINITION_REPRESENTATION(#4081,#4151);
#4063=SHAPE_DEFINITION_REPRESENTATION(#4082,#4152);
#4064=SHAPE_DEFINITION_REPRESENTATION(#4083,#4153);
#4065=SHAPE_DEFINITION_REPRESENTATION(#4084,#4154);
#4066=SHAPE_DEFINITION_REPRESENTATION(#4085,#4155);
#4067=SHAPE_DEFINITION_REPRESENTATION(#4086,#4156);
#4068=SHAPE_DEFINITION_REPRESENTATION(#4087,#4157);
#4069=SHAPE_DEFINITION_REPRESENTATION(#4088,#4158);
#4070=SHAPE_DEFINITION_REPRESENTATION(#4089,#4159);
#4071=SHAPE_DEFINITION_REPRESENTATION(#4090,#4160);
#4072=PRODUCT_DEFINITION_SHAPE('',$,#4162);
#4073=PRODUCT_DEFINITION_SHAPE('',$,#4163);
#4074=PRODUCT_DEFINITION_SHAPE('',$,#4164);
#4075=PRODUCT_DEFINITION_SHAPE('',$,#4165);
#4076=PRODUCT_DEFINITION_SHAPE('',$,#4166);
#4077=PRODUCT_DEFINITION_SHAPE('',$,#4167);
#4078=PRODUCT_DEFINITION_SHAPE('',$,#4168);
#4079=PRODUCT_DEFINITION_SHAPE('',$,#4169);
#4080=PRODUCT_DEFINITION_SHAPE('',$,#4170);
#4081=PRODUCT_DEFINITION_SHAPE('',$,#4171);
#4082=PRODUCT_DEFINITION_SHAPE('',$,#4172);
#4083=PRODUCT_DEFINITION_SHAPE('',$,#4173);
#4084=PRODUCT_DEFINITION_SHAPE('',$,#4174);
#4085=PRODUCT_DEFINITION_SHAPE('',$,#4175);
#4086=PRODUCT_DEFINITION_SHAPE('',$,#4176);
#4087=PRODUCT_DEFINITION_SHAPE('',$,#4177);
#4088=PRODUCT_DEFINITION_SHAPE('',$,#4178);
#4089=PRODUCT_DEFINITION_SHAPE('',$,#4179);
#4090=PRODUCT_DEFINITION_SHAPE('',$,#4180);
#4091=PRODUCT_DEFINITION_SHAPE($,$,#164);
#4092=PRODUCT_DEFINITION_SHAPE($,$,#165);
#4093=PRODUCT_DEFINITION_SHAPE($,$,#166);
#4094=PRODUCT_DEFINITION_SHAPE($,$,#167);
#4095=PRODUCT_DEFINITION_SHAPE($,$,#168);
#4096=PRODUCT_DEFINITION_SHAPE($,$,#169);
#4097=PRODUCT_DEFINITION_SHAPE($,$,#170);
#4098=PRODUCT_DEFINITION_SHAPE($,$,#171);
#4099=PRODUCT_DEFINITION_SHAPE($,$,#172);
#4100=PRODUCT_DEFINITION_SHAPE($,$,#173);
#4101=PRODUCT_DEFINITION_SHAPE($,$,#174);
#4102=PRODUCT_DEFINITION_SHAPE($,$,#175);
#4103=PRODUCT_DEFINITION_SHAPE($,$,#176);
#4104=PRODUCT_DEFINITION_SHAPE($,$,#177);
#4105=PRODUCT_DEFINITION_SHAPE($,$,#178);
#4106=PRODUCT_DEFINITION_SHAPE($,$,#179);
#4107=PRODUCT_DEFINITION_SHAPE($,$,#180);
#4108=PRODUCT_DEFINITION_SHAPE($,$,#181);
#4109=PRODUCT_DEFINITION_SHAPE($,$,#182);
#4110=PRODUCT_DEFINITION_SHAPE($,$,#183);
#4111=PRODUCT_DEFINITION_SHAPE($,$,#184);
#4112=PRODUCT_DEFINITION_SHAPE($,$,#185);
#4113=PRODUCT_DEFINITION_SHAPE($,$,#186);
#4114=PRODUCT_DEFINITION_SHAPE($,$,#187);
#4115=PRODUCT_DEFINITION_SHAPE($,$,#188);
#4116=PRODUCT_DEFINITION_SHAPE($,$,#189);
#4117=PRODUCT_DEFINITION_SHAPE($,$,#190);
#4118=PRODUCT_DEFINITION_SHAPE($,$,#191);
#4119=PRODUCT_DEFINITION_SHAPE($,$,#192);
#4120=PRODUCT_DEFINITION_SHAPE($,$,#193);
#4121=PRODUCT_DEFINITION_SHAPE($,$,#194);
#4122=PRODUCT_DEFINITION_SHAPE($,$,#195);
#4123=PRODUCT_DEFINITION_SHAPE($,$,#196);
#4124=PRODUCT_DEFINITION_SHAPE($,$,#197);
#4125=PRODUCT_DEFINITION_SHAPE($,$,#198);
#4126=PRODUCT_DEFINITION_SHAPE($,$,#199);
#4127=PRODUCT_DEFINITION_SHAPE($,$,#200);
#4128=PRODUCT_DEFINITION_SHAPE($,$,#201);
#4129=PRODUCT_DEFINITION_SHAPE($,$,#202);
#4130=PRODUCT_DEFINITION_SHAPE($,$,#203);
#4131=PRODUCT_DEFINITION_SHAPE($,$,#204);
#4132=PRODUCT_DEFINITION_SHAPE($,$,#205);
#4133=PRODUCT_DEFINITION_SHAPE($,$,#206);
#4134=PRODUCT_DEFINITION_SHAPE($,$,#207);
#4135=PRODUCT_DEFINITION_SHAPE($,$,#208);
#4136=PRODUCT_DEFINITION_SHAPE($,$,#209);
#4137=PRODUCT_DEFINITION_SHAPE($,$,#210);
#4138=PRODUCT_DEFINITION_SHAPE($,$,#211);
#4139=PRODUCT_DEFINITION_SHAPE($,$,#212);
#4140=PRODUCT_DEFINITION_SHAPE($,$,#213);
#4141=PRODUCT_DEFINITION_SHAPE($,$,#214);
#4142=SHAPE_REPRESENTATION('',(#2361,#2620,#2621,#2622,#2623,#2624,#2625,
#2626,#2627,#2628,#2629,#2630,#2631,#2632,#2633,#2634,#2635,#2636,#2637,
#2638,#2639,#2640,#2641,#2642,#2643,#2644,#2645,#2646,#2647,#2648,#2649,
#2650,#2651,#2652,#2653,#2654,#2655,#2656,#2657,#2658,#2659,#2660,#2661,
#2662,#2663,#2664,#2665,#2666,#2667,#2668,#2669,#2670),#4029);
#4143=SHAPE_REPRESENTATION('',(#2362),#4030);
#4144=SHAPE_REPRESENTATION('',(#2381),#4031);
#4145=SHAPE_REPRESENTATION('',(#2399),#4032);
#4146=SHAPE_REPRESENTATION('',(#2416),#4033);
#4147=SHAPE_REPRESENTATION('',(#2433),#4034);
#4148=SHAPE_REPRESENTATION('',(#2453),#4035);
#4149=SHAPE_REPRESENTATION('',(#2470),#4036);
#4150=SHAPE_REPRESENTATION('',(#2487),#4037);
#4151=SHAPE_REPRESENTATION('',(#2493),#4038);
#4152=SHAPE_REPRESENTATION('',(#2502),#4039);
#4153=SHAPE_REPRESENTATION('',(#2520),#4040);
#4154=SHAPE_REPRESENTATION('',(#2537),#4041);
#4155=SHAPE_REPRESENTATION('',(#2546),#4042);
#4156=SHAPE_REPRESENTATION('',(#2564),#4043);
#4157=SHAPE_REPRESENTATION('',(#2573),#4044);
#4158=SHAPE_REPRESENTATION('',(#2584),#4045);
#4159=SHAPE_REPRESENTATION('',(#2602),#4046);
#4160=SHAPE_REPRESENTATION('',(#2611),#4047);
#4161=PRODUCT_DEFINITION_CONTEXT('part definition',#4220,'design');
#4162=PRODUCT_DEFINITION('MAS-229','MAS-229',#4181,#4161);
#4163=PRODUCT_DEFINITION('Base plate','Base plate',#4182,#4161);
#4164=PRODUCT_DEFINITION('Support frame','Support frame',#4183,#4161);
#4165=PRODUCT_DEFINITION('Driving crank','Driving crank',#4184,#4161);
#4166=PRODUCT_DEFINITION('Upper rocker','Upper rocker',#4185,#4161);
#4167=PRODUCT_DEFINITION('Connecting link','Connecting link',#4186,#4161);
#4168=PRODUCT_DEFINITION('Lower rocker','Lower rocker',#4187,#4161);
#4169=PRODUCT_DEFINITION('Leg','Leg',#4188,#4161);
#4170=PRODUCT_DEFINITION('Foot pad','Foot pad',#4189,#4161);
#4171=PRODUCT_DEFINITION('Pivot bushing','Pivot bushing',#4190,#4161);
#4172=PRODUCT_DEFINITION('Ground pivot pin','Ground pivot pin',#4191,#4161);
#4173=PRODUCT_DEFINITION('Ground spacer','Ground spacer',#4192,#4161);
#4174=PRODUCT_DEFINITION('Pivot washer','Pivot washer',#4193,#4161);
#4175=PRODUCT_DEFINITION('Knee pivot pin','Knee pivot pin',#4194,#4161);
#4176=PRODUCT_DEFINITION('Knee spacer','Knee spacer',#4195,#4161);
#4177=PRODUCT_DEFINITION('Pivot retaining ring','Pivot retaining ring',
#4196,#4161);
#4178=PRODUCT_DEFINITION('Link pivot pin','Link pivot pin',#4197,#4161);
#4179=PRODUCT_DEFINITION('Back thrust washer','Back thrust washer',#4198,
#4161);
#4180=PRODUCT_DEFINITION('Link spacer','Link spacer',#4199,#4161);
#4181=PRODUCT_DEFINITION_FORMATION('',$,#4222);
#4182=PRODUCT_DEFINITION_FORMATION('',$,#4223);
#4183=PRODUCT_DEFINITION_FORMATION('',$,#4224);
#4184=PRODUCT_DEFINITION_FORMATION('',$,#4225);
#4185=PRODUCT_DEFINITION_FORMATION('',$,#4226);
#4186=PRODUCT_DEFINITION_FORMATION('',$,#4227);
#4187=PRODUCT_DEFINITION_FORMATION('',$,#4228);
#4188=PRODUCT_DEFINITION_FORMATION('',$,#4229);
#4189=PRODUCT_DEFINITION_FORMATION('',$,#4230);
#4190=PRODUCT_DEFINITION_FORMATION('',$,#4231);
#4191=PRODUCT_DEFINITION_FORMATION('',$,#4232);
#4192=PRODUCT_DEFINITION_FORMATION('',$,#4233);
#4193=PRODUCT_DEFINITION_FORMATION('',$,#4234);
#4194=PRODUCT_DEFINITION_FORMATION('',$,#4235);
#4195=PRODUCT_DEFINITION_FORMATION('',$,#4236);
#4196=PRODUCT_DEFINITION_FORMATION('',$,#4237);
#4197=PRODUCT_DEFINITION_FORMATION('',$,#4238);
#4198=PRODUCT_DEFINITION_FORMATION('',$,#4239);
#4199=PRODUCT_DEFINITION_FORMATION('',$,#4240);
#4200=PRODUCT_RELATED_PRODUCT_CATEGORY('MAS-229','MAS-229',(#4222));
#4201=PRODUCT_RELATED_PRODUCT_CATEGORY('Base plate','Base plate',(#4223));
#4202=PRODUCT_RELATED_PRODUCT_CATEGORY('Support frame','Support frame',
(#4224));
#4203=PRODUCT_RELATED_PRODUCT_CATEGORY('Driving crank','Driving crank',
(#4225));
#4204=PRODUCT_RELATED_PRODUCT_CATEGORY('Upper rocker','Upper rocker',(#4226));
#4205=PRODUCT_RELATED_PRODUCT_CATEGORY('Connecting link',
'Connecting link',(#4227));
#4206=PRODUCT_RELATED_PRODUCT_CATEGORY('Lower rocker','Lower rocker',(#4228));
#4207=PRODUCT_RELATED_PRODUCT_CATEGORY('Leg','Leg',(#4229));
#4208=PRODUCT_RELATED_PRODUCT_CATEGORY('Foot pad','Foot pad',(#4230));
#4209=PRODUCT_RELATED_PRODUCT_CATEGORY('Pivot bushing','Pivot bushing',
(#4231));
#4210=PRODUCT_RELATED_PRODUCT_CATEGORY('Ground pivot pin',
'Ground pivot pin',(#4232));
#4211=PRODUCT_RELATED_PRODUCT_CATEGORY('Ground spacer','Ground spacer',
(#4233));
#4212=PRODUCT_RELATED_PRODUCT_CATEGORY('Pivot washer','Pivot washer',(#4234));
#4213=PRODUCT_RELATED_PRODUCT_CATEGORY('Knee pivot pin',
'Knee pivot pin',(#4235));
#4214=PRODUCT_RELATED_PRODUCT_CATEGORY('Knee spacer','Knee spacer',(#4236));
#4215=PRODUCT_RELATED_PRODUCT_CATEGORY('Pivot retaining ring',
'Pivot retaining ring',(#4237));
#4216=PRODUCT_RELATED_PRODUCT_CATEGORY('Link pivot pin',
'Link pivot pin',(#4238));
#4217=PRODUCT_RELATED_PRODUCT_CATEGORY('Back thrust washer',
'Back thrust washer',(#4239));
#4218=PRODUCT_RELATED_PRODUCT_CATEGORY('Link spacer','Link spacer',(#4240));
#4219=APPLICATION_PROTOCOL_DEFINITION('international standard',
'automotive_design',2009,#4220);
#4220=APPLICATION_CONTEXT(
'Core Data for Automotive Mechanical Design Process');
#4221=PRODUCT_CONTEXT('part definition',#4220,'mechanical');
#4222=PRODUCT('MAS-229','MAS-229',
'Independently dimensioned six-bar single-leg walking-linkage demonstr
ator. Whole-mm20 crank,60 upper rocker,80/120 ternary coupler,120 lowe
r rocker,140 knee pitch and260 toe reach; ground pivots0/0,60/0,40/60.
 Seven native revolutes close both loops. Four reused native library f
amilies, fully retained shared pins and layered real spacer stacks, bo
nded rubber toe. Benchtop reference mechanism; no complete vehicle, lo
ad, gait stability, adhesive, weld, fit or life rating.',(#4221));
#4223=PRODUCT('Base plate','Base plate','Base plate',(#4221));
#4224=PRODUCT('Support frame','Support frame','Support frame',(#4221));
#4225=PRODUCT('Driving crank','Driving crank','Driving crank',(#4221));
#4226=PRODUCT('Upper rocker','Upper rocker',$,(#4221));
#4227=PRODUCT('Connecting link','Connecting link','Connecting link',(#4221));
#4228=PRODUCT('Lower rocker','Lower rocker',$,(#4221));
#4229=PRODUCT('Leg','Leg',$,(#4221));
#4230=PRODUCT('Foot pad','Foot pad','Foot pad',(#4221));
#4231=PRODUCT('Pivot bushing','Pivot bushing',$,(#4221));
#4232=PRODUCT('Ground pivot pin','Ground pivot pin',$,(#4221));
#4233=PRODUCT('Ground spacer','Ground spacer',
'Turn OD, drill bore, face to length. Nominal dimensions in mm. Fit li
mits to be assigned at assembly level.',(#4221));
#4234=PRODUCT('Pivot washer','Pivot washer',$,(#4221));
#4235=PRODUCT('Knee pivot pin','Knee pivot pin',$,(#4221));
#4236=PRODUCT('Knee spacer','Knee spacer',$,(#4221));
#4237=PRODUCT('Pivot retaining ring','Pivot retaining ring',$,(#4221));
#4238=PRODUCT('Link pivot pin','Link pivot pin',$,(#4221));
#4239=PRODUCT('Back thrust washer','Back thrust washer',$,(#4221));
#4240=PRODUCT('Link spacer','Link spacer','Link spacer',(#4221));
#4241=PRESENTATION_STYLE_ASSIGNMENT((#4255));
#4242=PRESENTATION_STYLE_ASSIGNMENT((#4256));
#4243=PRESENTATION_STYLE_ASSIGNMENT((#4257));
#4244=PRESENTATION_STYLE_ASSIGNMENT((#4258));
#4245=PRESENTATION_STYLE_ASSIGNMENT((#4259));
#4246=PRESENTATION_STYLE_ASSIGNMENT((#4260));
#4247=PRESENTATION_STYLE_ASSIGNMENT((#4261));
#4248=PRESENTATION_STYLE_ASSIGNMENT((#4262));
#4249=PRESENTATION_STYLE_ASSIGNMENT((#4263));
#4250=PRESENTATION_STYLE_ASSIGNMENT((#4264));
#4251=PRESENTATION_STYLE_ASSIGNMENT((#4265));
#4252=PRESENTATION_STYLE_ASSIGNMENT((#4266));
#4253=PRESENTATION_STYLE_ASSIGNMENT((#4267));
#4254=PRESENTATION_STYLE_ASSIGNMENT((#4268));
#4255=SURFACE_STYLE_USAGE(.BOTH.,#4269);
#4256=SURFACE_STYLE_USAGE(.BOTH.,#4270);
#4257=SURFACE_STYLE_USAGE(.BOTH.,#4271);
#4258=SURFACE_STYLE_USAGE(.BOTH.,#4272);
#4259=SURFACE_STYLE_USAGE(.BOTH.,#4273);
#4260=SURFACE_STYLE_USAGE(.BOTH.,#4274);
#4261=SURFACE_STYLE_USAGE(.BOTH.,#4275);
#4262=SURFACE_STYLE_USAGE(.BOTH.,#4276);
#4263=SURFACE_STYLE_USAGE(.BOTH.,#4277);
#4264=SURFACE_STYLE_USAGE(.BOTH.,#4278);
#4265=SURFACE_STYLE_USAGE(.BOTH.,#4279);
#4266=SURFACE_STYLE_USAGE(.BOTH.,#4280);
#4267=SURFACE_STYLE_USAGE(.BOTH.,#4281);
#4268=SURFACE_STYLE_USAGE(.BOTH.,#4282);
#4269=SURFACE_SIDE_STYLE('',(#4283));
#4270=SURFACE_SIDE_STYLE('',(#4284));
#4271=SURFACE_SIDE_STYLE('',(#4285));
#4272=SURFACE_SIDE_STYLE('',(#4286));
#4273=SURFACE_SIDE_STYLE('',(#4287));
#4274=SURFACE_SIDE_STYLE('',(#4288));
#4275=SURFACE_SIDE_STYLE('',(#4289));
#4276=SURFACE_SIDE_STYLE('',(#4290));
#4277=SURFACE_SIDE_STYLE('',(#4291));
#4278=SURFACE_SIDE_STYLE('',(#4292));
#4279=SURFACE_SIDE_STYLE('',(#4293));
#4280=SURFACE_SIDE_STYLE('',(#4294));
#4281=SURFACE_SIDE_STYLE('',(#4295));
#4282=SURFACE_SIDE_STYLE('',(#4296));
#4283=SURFACE_STYLE_FILL_AREA(#4297);
#4284=SURFACE_STYLE_FILL_AREA(#4298);
#4285=SURFACE_STYLE_FILL_AREA(#4299);
#4286=SURFACE_STYLE_FILL_AREA(#4300);
#4287=SURFACE_STYLE_FILL_AREA(#4301);
#4288=SURFACE_STYLE_FILL_AREA(#4302);
#4289=SURFACE_STYLE_FILL_AREA(#4303);
#4290=SURFACE_STYLE_FILL_AREA(#4304);
#4291=SURFACE_STYLE_FILL_AREA(#4305);
#4292=SURFACE_STYLE_FILL_AREA(#4306);
#4293=SURFACE_STYLE_FILL_AREA(#4307);
#4294=SURFACE_STYLE_FILL_AREA(#4308);
#4295=SURFACE_STYLE_FILL_AREA(#4309);
#4296=SURFACE_STYLE_FILL_AREA(#4310);
#4297=FILL_AREA_STYLE('Steel - Satin',(#4311));
#4298=FILL_AREA_STYLE('Dark blue',(#4312));
#4299=FILL_AREA_STYLE('Frame gray',(#4313));
#4300=FILL_AREA_STYLE('Driving crank finish',(#4314));
#4301=FILL_AREA_STYLE('Upper rocker finish',(#4315));
#4302=FILL_AREA_STYLE('Connecting link finish',(#4316));
#4303=FILL_AREA_STYLE('Lower rocker finish',(#4317));
#4304=FILL_AREA_STYLE('Leg finish',(#4318));
#4305=FILL_AREA_STYLE('Foot charcoal',(#4319));
#4306=FILL_AREA_STYLE('Bearing light gray',(#4320));
#4307=FILL_AREA_STYLE('Pin gray',(#4321));
#4308=FILL_AREA_STYLE('Washer light gray',(#4322));
#4309=FILL_AREA_STYLE('Spacer gray',(#4323));
#4310=FILL_AREA_STYLE('Dark gray',(#4324));
#4311=FILL_AREA_STYLE_COLOUR('Steel - Satin',#4325);
#4312=FILL_AREA_STYLE_COLOUR('Dark blue',#4326);
#4313=FILL_AREA_STYLE_COLOUR('Frame gray',#4327);
#4314=FILL_AREA_STYLE_COLOUR('Driving crank finish',#4328);
#4315=FILL_AREA_STYLE_COLOUR('Upper rocker finish',#4329);
#4316=FILL_AREA_STYLE_COLOUR('Connecting link finish',#4330);
#4317=FILL_AREA_STYLE_COLOUR('Lower rocker finish',#4331);
#4318=FILL_AREA_STYLE_COLOUR('Leg finish',#4332);
#4319=FILL_AREA_STYLE_COLOUR('Foot charcoal',#4333);
#4320=FILL_AREA_STYLE_COLOUR('Bearing light gray',#4334);
#4321=FILL_AREA_STYLE_COLOUR('Pin gray',#4335);
#4322=FILL_AREA_STYLE_COLOUR('Washer light gray',#4336);
#4323=FILL_AREA_STYLE_COLOUR('Spacer gray',#4337);
#4324=FILL_AREA_STYLE_COLOUR('Dark gray',#4338);
#4325=COLOUR_RGB('Steel - Satin',0.627450980392157,0.627450980392157,0.627450980392157);
#4326=COLOUR_RGB('Dark blue',0.0901960784313725,0.270588235294118,0.513725490196078);
#4327=COLOUR_RGB('Frame gray',0.407843137254902,0.447058823529412,0.498039215686275);
#4328=COLOUR_RGB('Driving crank finish',0.0901960784313725,0.270588235294118,
0.513725490196078);
#4329=COLOUR_RGB('Upper rocker finish',0.317647058823529,0.686274509803922,
0.890196078431372);
#4330=COLOUR_RGB('Connecting link finish',0.662745098039216,0.831372549019608,
0.949019607843137);
#4331=COLOUR_RGB('Lower rocker finish',0.317647058823529,0.686274509803922,
0.890196078431372);
#4332=COLOUR_RGB('Leg finish',0.0901960784313725,0.270588235294118,0.513725490196078);
#4333=COLOUR_RGB('Foot charcoal',0.164705882352941,0.184313725490196,0.211764705882353);
#4334=COLOUR_RGB('Bearing light gray',0.725490196078431,0.752941176470588,
0.792156862745098);
#4335=COLOUR_RGB('Pin gray',0.576470588235294,0.615686274509804,0.666666666666667);
#4336=COLOUR_RGB('Washer light gray',0.725490196078431,0.752941176470588,
0.792156862745098);
#4337=COLOUR_RGB('Spacer gray',0.576470588235294,0.615686274509804,0.666666666666667);
#4338=COLOUR_RGB('Dark gray',0.250980392156863,0.282352941176471,0.32156862745098);
ENDSEC;
END-ISO-10303-21;
